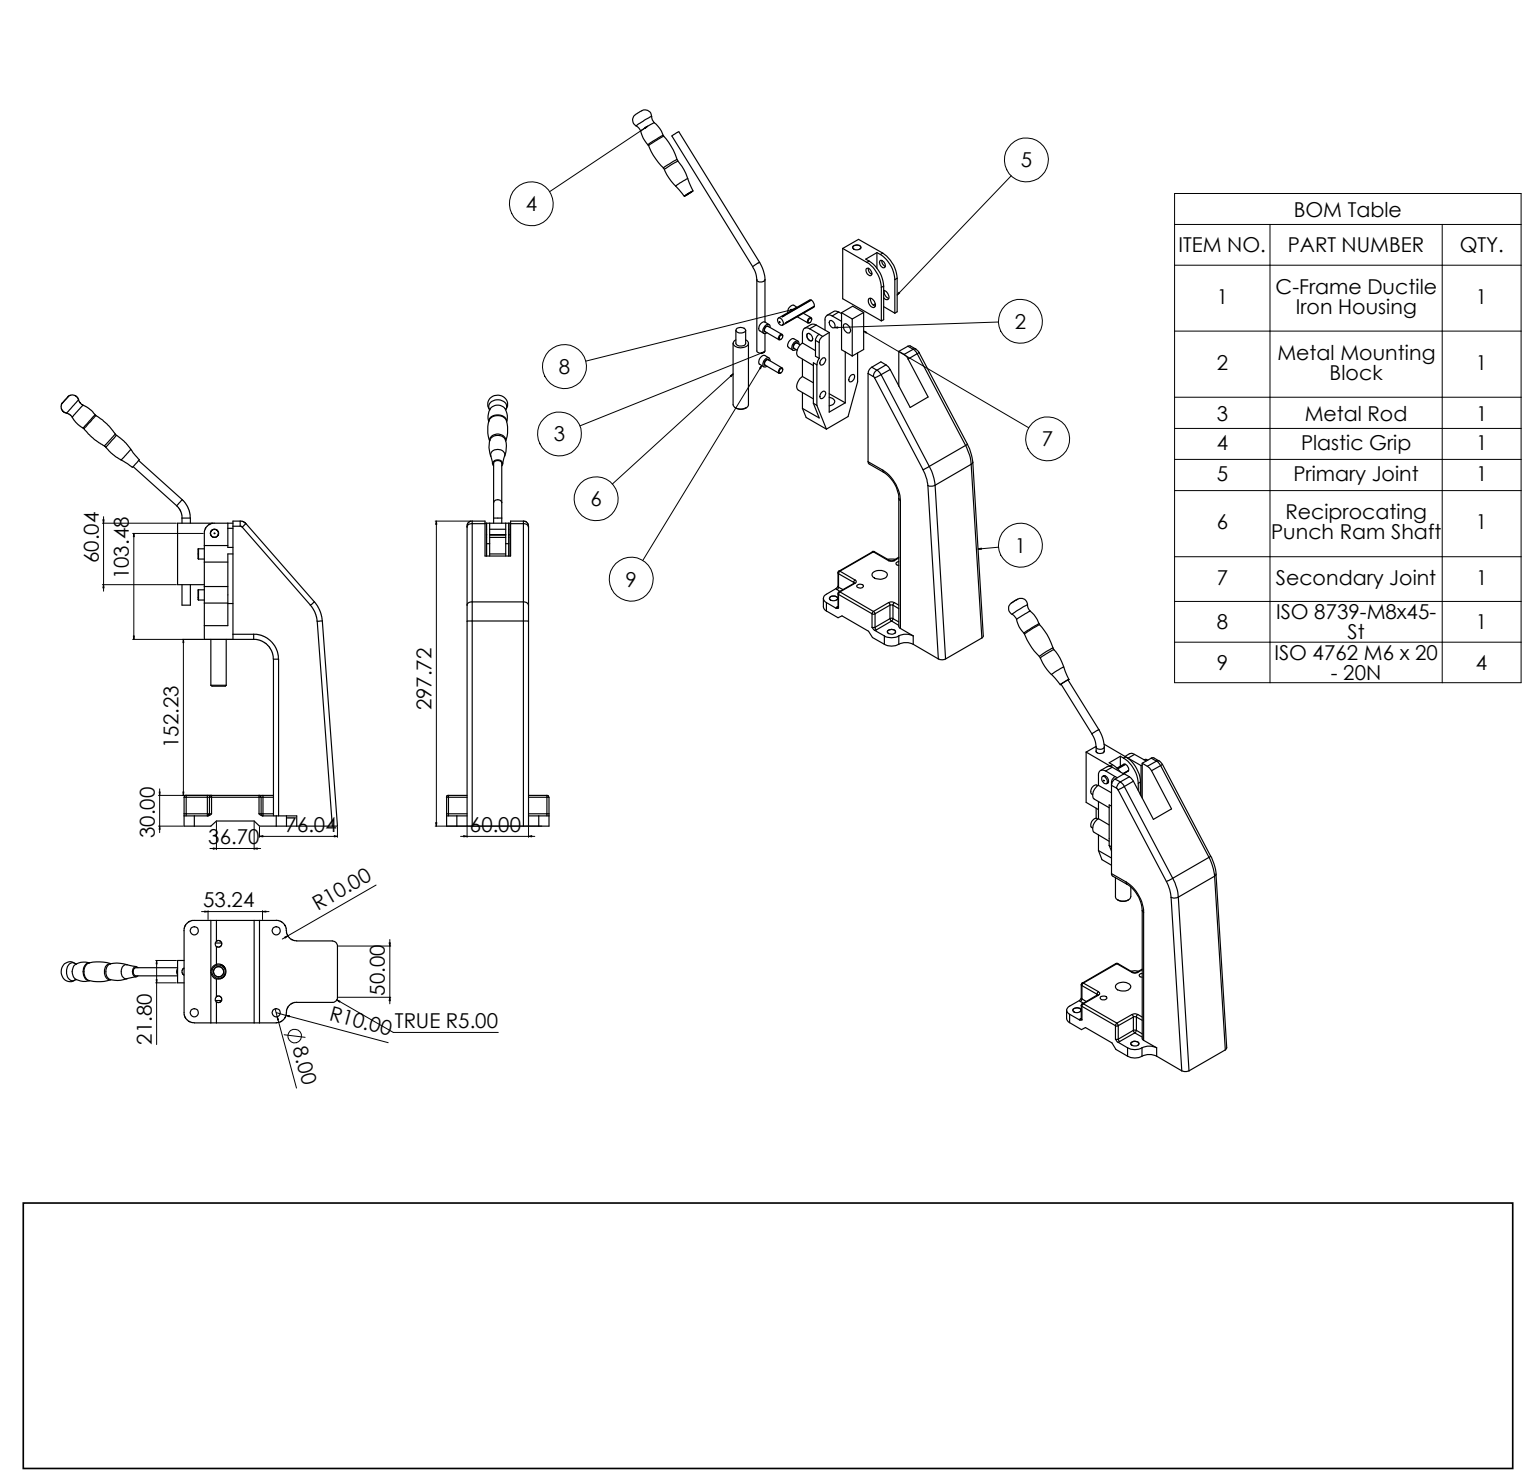
ISO-10303-21;
HEADER;
FILE_DESCRIPTION (('STEP AP214'),
    '1' );
FILE_NAME ('MAS-316',
    '2026-10-20T14:49:59',
    ( '' ),
    ( '' ),
    'SwSTEP 2.0',
    'SolidWorks 2025',
    '' );
FILE_SCHEMA (( 'AUTOMOTIVE_DESIGN' ));
ENDSEC;

DATA;
#1 = AXIS2_PLACEMENT_3D ( 'NONE', #1947, #6240, #1422 ) ;
#2 = CARTESIAN_POINT ( 'NONE',  ( 3.000000000000000000, 2.935248768560057897, -3.252606517456513302E-15 ) ) ;
#3 = LINE ( 'NONE', #5660, #7079 ) ;
#4 = DIRECTION ( 'NONE',  ( -0.6691306063588561281, -0.7431448254773960205, 0.000000000000000000 ) ) ;
#5 =( BOUNDED_CURVE ( )  B_SPLINE_CURVE ( 3, ( #4259, #2824, #7496, #242 ),
 .UNSPECIFIED., .F., .F. ) 
 B_SPLINE_CURVE_WITH_KNOTS ( ( 4, 4 ),
 ( 3.228493165690314637, 4.434806757669079502 ),
 .UNSPECIFIED. ) 
 CURVE ( )  GEOMETRIC_REPRESENTATION_ITEM ( )  RATIONAL_B_SPLINE_CURVE ( ( 1.000000000000000000, 0.8823660295963204891, 0.8823660295963204891, 1.000000000000000000 ) ) 
 REPRESENTATION_ITEM ( '' )  );
#6 = ORIENTED_EDGE ( 'NONE', *, *, #7618, .F. ) ;
#7 = EDGE_CURVE ( 'NONE', #389, #4565, #2197, .T. ) ;
#8 = VERTEX_POINT ( 'NONE', #6223 ) ;
#9 = ORIENTED_EDGE ( 'NONE', *, *, #9037, .T. ) ;
#10 = FACE_BOUND ( 'NONE', #10352, .T. ) ;
#11 = CARTESIAN_POINT ( 'NONE',  ( -47.94539818030330025, 137.0132282531173473, 3.999999999999991562 ) ) ;
#12 = DIRECTION ( 'NONE',  ( 0.000000000000000000, 0.000000000000000000, 1.000000000000000000 ) ) ;
#13 = VERTEX_POINT ( 'NONE', #5217 ) ;
#14 = DIRECTION ( 'NONE',  ( -0.6691306063588562392, -0.7431448254773959095, 0.000000000000000000 ) ) ;
#15 = ORIENTED_EDGE ( 'NONE', *, *, #8479, .F. ) ;
#16 = DIRECTION ( 'NONE',  ( -0.6691306063588565722, -0.7431448254773957984, 0.000000000000000000 ) ) ;
#17 = EDGE_CURVE ( 'NONE', #7054, #8863, #10257, .T. ) ;
#18 = ORIENTED_EDGE ( 'NONE', *, *, #2489, .T. ) ;
#19 = VECTOR ( 'NONE', #6137, 1000.000000000000114 ) ;
#20 = ORIENTED_EDGE ( 'NONE', *, *, #4444, .T. ) ;
#21 = DIRECTION ( 'NONE',  ( -1.000000000000000000, 0.000000000000000000, -1.396588258780021135E-16 ) ) ;
#22 = FACE_OUTER_BOUND ( 'NONE', #5382, .T. ) ;
#23 = PRODUCT_DEFINITION_SHAPE ( 'NONE', 'NONE',  #10488 ) ;
#24 = DIRECTION ( 'NONE',  ( 0.000000000000000000, -1.000000000000000000, -9.100899318238107179E-17 ) ) ;
#25 = DIRECTION ( 'NONE',  ( -1.000000000000000000, 0.000000000000000000, 0.000000000000000000 ) ) ;
#26 = AXIS2_PLACEMENT_3D ( 'NONE', #141, #5845, #6542 ) ;
#27 = ORIENTED_EDGE ( 'NONE', *, *, #3979, .T. ) ;
#28 = VECTOR ( 'NONE', #9785, 1000.000000000000000 ) ;
#29 = CARTESIAN_POINT ( 'NONE',  ( 3.000000000000000000, 0.000000000000000000, 0.000000000000000000 ) ) ;
#30 = ADVANCED_FACE ( 'NONE', ( #9249 ), #6112, .F. ) ;
#31 = EDGE_CURVE ( 'NONE', #2894, #7105, #9463, .T. ) ;
#32 = EDGE_CURVE ( 'NONE', #6206, #5311, #7708, .T. ) ;
#33 = CONTEXT_DEPENDENT_SHAPE_REPRESENTATION ( #9797, #23 ) ;
#34 = VERTEX_POINT ( 'NONE', #5261 ) ;
#35 = DIRECTION ( 'NONE',  ( 1.000000000000000000, -0.000000000000000000, -0.000000000000000000 ) ) ;
#36 = VERTEX_POINT ( 'NONE', #6165 ) ;
#37 = CIRCLE ( 'NONE', #7311, 10.00000000000000178 ) ;
#38 = AXIS2_PLACEMENT_3D ( 'NONE', #7742, #2701, #6091 ) ;
#39 = VERTEX_POINT ( 'NONE', #5423 ) ;
#40 = CARTESIAN_POINT ( 'NONE',  ( 2.108096605167895612E-14, -117.1457019118819005, -25.15769640663941686 ) ) ;
#41 = CARTESIAN_POINT ( 'NONE',  ( -7.293506896408097795, 145.5696653505793563, -20.00000000000000711 ) ) ;
#42 = CARTESIAN_POINT ( 'NONE',  ( 39.99999999999998579, -135.1707019118818778, -36.00000000000002842 ) ) ;
#43 = DIRECTION ( 'NONE',  ( -1.000000000000000000, 0.000000000000000000, 0.000000000000000000 ) ) ;
#44 = LINE ( 'NONE', #8251, #3603 ) ;
#45 = VECTOR ( 'NONE', #8925, 1000.000000000000000 ) ;
#46 = EDGE_CURVE ( 'NONE', #9808, #836, #8928, .T. ) ;
#47 = VERTEX_POINT ( 'NONE', #6006 ) ;
#48 = CARTESIAN_POINT ( 'NONE',  ( -16.29350689640809691, -186.9457019118818835, 23.72119897386845722 ) ) ;
#49 = ORIENTED_EDGE ( 'NONE', *, *, #1262, .T. ) ;
#50 = DIRECTION ( 'NONE',  ( 1.000000000000000000, 0.000000000000000000, -1.734723475976805615E-16 ) ) ;
#51 = CYLINDRICAL_SURFACE ( 'NONE', #8825, 4.000000000000000000 ) ;
#52 = AXIS2_PLACEMENT_3D ( 'NONE', #3037, #3895, #4040 ) ;
#53 =( NAMED_UNIT ( * ) SI_UNIT ( $, .STERADIAN. ) SOLID_ANGLE_UNIT ( ) );
#54 = AXIS2_PLACEMENT_3D ( 'NONE', #4576, #604, #662 ) ;
#55 = DIRECTION ( 'NONE',  ( -0.7367503238654704578, -0.6761648913424330720, -0.000000000000000000 ) ) ;
#56 = CARTESIAN_POINT ( 'NONE',  ( 99.80027788547049283, -145.1457019118819574, 25.00000000000000000 ) ) ;
#57 = LINE ( 'NONE', #8266, #434 ) ;
#58 = ORIENTED_EDGE ( 'NONE', *, *, #5513, .T. ) ;
#59 = VERTEX_POINT ( 'NONE', #6862 ) ;
#60 = ORIENTED_EDGE ( 'NONE', *, *, #10146, .T. ) ;
#61 = AXIS2_PLACEMENT_3D ( 'NONE', #1587, #8044, #3822 ) ;
#62 = ORIENTED_EDGE ( 'NONE', *, *, #3204, .F. ) ;
#63 = CARTESIAN_POINT ( 'NONE',  ( -47.94539818030330025, 150.5696653505793563, 3.999999999999993339 ) ) ;
#64 = ADVANCED_FACE ( 'NONE', ( #10099 ), #3860, .F. ) ;
#65 = DIRECTION ( 'NONE',  ( -0.000000000000000000, -0.000000000000000000, -1.000000000000000000 ) ) ;
#66 = LINE ( 'NONE', #8964, #2259 ) ;
#67 = DIRECTION ( 'NONE',  ( -0.7071067811864983899, 8.659560562354331352E-17, 0.7071067811865966446 ) ) ;
#68 = CIRCLE ( 'NONE', #1421, 4.025000000000000355 ) ;
#69 = ORIENTED_EDGE ( 'NONE', *, *, #7396, .F. ) ;
#70 = FACE_OUTER_BOUND ( 'NONE', #3100, .T. ) ;
#71 = VECTOR ( 'NONE', #3438, 1000.000000000000000 ) ;
#72 = ORIENTED_EDGE ( 'NONE', *, *, #1454, .F. ) ;
#73 = CIRCLE ( 'NONE', #8358, 4.025000000000000355 ) ;
#74 = ORIENTED_EDGE ( 'NONE', *, *, #80, .F. ) ;
#75 = UNCERTAINTY_MEASURE_WITH_UNIT (LENGTH_MEASURE( 1.000000000000000082E-05 ), #6894, 'distance_accuracy_value', 'NONE');
#76 = ORIENTED_EDGE ( 'NONE', *, *, #6234, .T. ) ;
#77 = DIRECTION ( 'NONE',  ( -1.000000000000000000, 0.000000000000000000, 0.000000000000000000 ) ) ;
#78 = DIRECTION ( 'NONE',  ( 0.000000000000000000, 1.000000000000000000, -1.329743448921560837E-15 ) ) ;
#79 = LINE ( 'NONE', #3304, #8495 ) ;
#80 = EDGE_CURVE ( 'NONE', #1253, #6094, #1141, .T. ) ;
#81 = DIRECTION ( 'NONE',  ( 0.000000000000000000, 1.000000000000000000, 0.000000000000000000 ) ) ;
#82 = LINE ( 'NONE', #7283, #1628 ) ;
#83 = CIRCLE ( 'NONE', #590, 5.025000000000002132 ) ;
#84 = VERTEX_POINT ( 'NONE', #3844 ) ;
#85 = DIRECTION ( 'NONE',  ( 0.000000000000000000, 0.000000000000000000, -1.000000000000000000 ) ) ;
#86 = VERTEX_POINT ( 'NONE', #4732 ) ;
#87 = CARTESIAN_POINT ( 'NONE',  ( 37.22511195853866894, 17.84145331825995484, -25.00000000000000355 ) ) ;
#88 = ORIENTED_EDGE ( 'NONE', *, *, #32, .T. ) ;
#89 = ADVANCED_FACE ( 'NONE', ( #9520 ), #9630, .T. ) ;
#90 = ADVANCED_FACE ( 'NONE', ( #4832 ), #5200, .F. ) ;
#91 = DIRECTION ( 'NONE',  ( 0.000000000000000000, -1.222897680782651471E-16, 1.000000000000000000 ) ) ;
#92 = AXIS2_PLACEMENT_3D ( 'NONE', #1690, #1849, #8953 ) ;
#93 = DIRECTION ( 'NONE',  ( 0.000000000000000000, -0.000000000000000000, -1.000000000000000000 ) ) ;
#94 = FACE_OUTER_BOUND ( 'NONE', #233, .T. ) ;
#95 = DIRECTION ( 'NONE',  ( -0.000000000000000000, -0.000000000000000000, 1.000000000000000000 ) ) ;
#96 = DIRECTION ( 'NONE',  ( 0.000000000000000000, 0.000000000000000000, 1.000000000000000000 ) ) ;
#97 = EDGE_LOOP ( 'NONE', ( #5379, #7947, #3762, #7012 ) ) ;
#98 = LINE ( 'NONE', #6716, #4014 ) ;
#99 = ORIENTED_EDGE ( 'NONE', *, *, #5544, .F. ) ;
#100 = LINE ( 'NONE', #5018, #2677 ) ;
#101 = EDGE_CURVE ( 'NONE', #6753, #3816, #8421, .T. ) ;
#102 = CYLINDRICAL_SURFACE ( 'NONE', #1212, 2.000000000000001776 ) ;
#103 = EDGE_CURVE ( 'NONE', #7113, #7038, #645, .T. ) ;
#104 = VECTOR ( 'NONE', #4491, 1000.000000000000000 ) ;
#105 = EDGE_CURVE ( 'NONE', #8005, #7120, #1404, .T. ) ;
#106 = DIRECTION ( 'NONE',  ( -1.000000000000000000, -0.000000000000000000, -0.000000000000000000 ) ) ;
#107 = DIRECTION ( 'NONE',  ( 0.000000000000000000, 0.000000000000000000, 1.000000000000000000 ) ) ;
#108 = DIRECTION ( 'NONE',  ( 1.000000000000000000, 0.000000000000000000, 0.000000000000000000 ) ) ;
#109 = VERTEX_POINT ( 'NONE', #7181 ) ;
#110 = ORIENTED_EDGE ( 'NONE', *, *, #8315, .T. ) ;
#111 = ORIENTED_EDGE ( 'NONE', *, *, #371, .T. ) ;
#112 = AXIS2_PLACEMENT_3D ( 'NONE', #10075, #7738, #3660 ) ;
#113 = VECTOR ( 'NONE', #5634, 1000.000000000000000 ) ;
#114 = ORIENTED_EDGE ( 'NONE', *, *, #3993, .T. ) ;
#115 = ORIENTED_EDGE ( 'NONE', *, *, #7748, .F. ) ;
#116 = DIRECTION ( 'NONE',  ( 0.000000000000000000, 0.000000000000000000, 1.000000000000000000 ) ) ;
#117 =( NAMED_UNIT ( * ) SI_UNIT ( $, .STERADIAN. ) SOLID_ANGLE_UNIT ( ) );
#118 = EDGE_CURVE ( 'NONE', #991, #7873, #6383, .T. ) ;
#119 = DIRECTION ( 'NONE',  ( -0.000000000000000000, 1.000000000000000000, -0.000000000000000000 ) ) ;
#120 = DIRECTION ( 'NONE',  ( -0.000000000000000000, 1.000000000000000000, -0.000000000000000000 ) ) ;
#121 = VECTOR ( 'NONE', #5228, 1000.000000000000000 ) ;
#122 = ORIENTED_EDGE ( 'NONE', *, *, #3348, .T. ) ;
#123 = DIRECTION ( 'NONE',  ( -0.000000000000000000, 1.000000000000000000, -0.000000000000000000 ) ) ;
#124 = CIRCLE ( 'NONE', #1803, 7.500000000000000000 ) ;
#125 = VERTEX_POINT ( 'NONE', #7868 ) ;
#126 = VECTOR ( 'NONE', #3375, 1000.000000000000000 ) ;
#127 = CARTESIAN_POINT ( 'NONE',  ( 39.99999999999998579, -115.1457019118818863, -50.00000000000002132 ) ) ;
#128 = EDGE_CURVE ( 'NONE', #9477, #9534, #1310, .T. ) ;
#129 = VECTOR ( 'NONE', #2614, 1000.000000000000000 ) ;
#130 = ORIENTED_EDGE ( 'NONE', *, *, #2088, .F. ) ;
#131 = ORIENTED_EDGE ( 'NONE', *, *, #6804, .F. ) ;
#132 = DIRECTION ( 'NONE',  ( -0.7431448254773957984, 0.6691306063588565722, -0.000000000000000000 ) ) ;
#133 = ADVANCED_BREP_SHAPE_REPRESENTATION ( '', ( #10321, #4601 ), #2278 ) ;
#134 = CIRCLE ( 'NONE', #4024, 3.999999999999993339 ) ;
#135 = DIRECTION ( 'NONE',  ( 0.000000000000000000, 0.000000000000000000, -1.000000000000000000 ) ) ;
#136 = CARTESIAN_POINT ( 'NONE',  ( -16.29350689640809691, -8.635287962196477096, 0.000000000000000000 ) ) ;
#137 = DIRECTION ( 'NONE',  ( 0.000000000000000000, 0.000000000000000000, 1.000000000000000000 ) ) ;
#138 = CARTESIAN_POINT ( 'NONE',  ( -7.293506896408097795, 50.54838324668256888, 20.00000000000001776 ) ) ;
#139 = VECTOR ( 'NONE', #10142, 1000.000000000000000 ) ;
#140 = ORIENTED_EDGE ( 'NONE', *, *, #5070, .F. ) ;
#141 = CARTESIAN_POINT ( 'NONE',  ( -23.17384457509314899, 130.5696653505793847, 10.90000000000000036 ) ) ;
#142 = EDGE_CURVE ( 'NONE', #5755, #3381, #6273, .T. ) ;
#143 = ORIENTED_EDGE ( 'NONE', *, *, #3330, .T. ) ;
#144 = DIRECTION ( 'NONE',  ( -1.000000000000000000, 0.000000000000000000, 0.000000000000000000 ) ) ;
#145 = ORIENTED_EDGE ( 'NONE', *, *, #5104, .T. ) ;
#146 = AXIS2_PLACEMENT_3D ( 'NONE', #654, #6367, #4769 ) ;
#147 = SHAPE_REPRESENTATION_RELATIONSHIP ( 'NONE' , 'NONE' ,  #7587, #133 ) ;
#148 = FACE_OUTER_BOUND ( 'NONE', #7245, .T. ) ;
#149 = AXIS2_PLACEMENT_3D ( 'NONE', #5640, #2363, #7980 ) ;
#150 = FACE_BOUND ( 'NONE', #8598, .T. ) ;
#151 = FACE_OUTER_BOUND ( 'NONE', #4068, .T. ) ;
#152 = FACE_OUTER_BOUND ( 'NONE', #4686, .T. ) ;
#153 = DIRECTION ( 'NONE',  ( -1.000000000000000000, 0.000000000000000000, 0.000000000000000000 ) ) ;
#154 = AXIS2_PLACEMENT_3D ( 'NONE', #9604, #3022, #736 ) ;
#155 = EDGE_CURVE ( 'NONE', #5994, #6514, #9956, .T. ) ;
#156 = ORIENTED_EDGE ( 'NONE', *, *, #9691, .F. ) ;
#157 = CARTESIAN_POINT ( 'NONE',  ( -2.293506896408097795, 120.5696653505793705, 20.00000000000000711 ) ) ;
#158 = CIRCLE ( 'NONE', #4883, 4.982234098198590644 ) ;
#159 = ORIENTED_EDGE ( 'NONE', *, *, #5597, .F. ) ;
#160 = CARTESIAN_POINT ( 'NONE',  ( -2.293506896408097795, 120.5696653505793705, 16.00000000000000711 ) ) ;
#161 = FACE_OUTER_BOUND ( 'NONE', #8002, .T. ) ;
#162 = DIRECTION ( 'NONE',  ( 0.000000000000000000, 0.000000000000000000, -1.000000000000000000 ) ) ;
#163 = CARTESIAN_POINT ( 'NONE',  ( 0.000000000000000000, -135.1457019118818721, 49.99999999999997868 ) ) ;
#164 = DIRECTION ( 'NONE',  ( -0.000000000000000000, 1.000000000000000000, -0.000000000000000000 ) ) ;
#165 = DIRECTION ( 'NONE',  ( 1.000000000000000000, 0.000000000000000000, -0.000000000000000000 ) ) ;
#166 = CONICAL_SURFACE ( 'NONE', #1514, 4.025000000000000355, 0.7853981633977258348 ) ;
#167 = ORIENTED_EDGE ( 'NONE', *, *, #1641, .F. ) ;
#168 = ADVANCED_FACE ( 'NONE', ( #10363, #4632, #9677 ), #1511, .F. ) ;
#169 = EDGE_CURVE ( 'NONE', #490, #9911, #7578, .T. ) ;
#170 = EDGE_LOOP ( 'NONE', ( #1521, #9934, #3722, #2301 ) ) ;
#171 = EDGE_CURVE ( 'NONE', #8144, #3030, #5631, .T. ) ;
#172 = VERTEX_POINT ( 'NONE', #5530 ) ;
#173 = DIRECTION ( 'NONE',  ( 1.000000000000000000, 0.000000000000000000, 0.000000000000000000 ) ) ;
#174 = CARTESIAN_POINT ( 'NONE',  ( 4.856471286862176662, 145.0444252872335937, -25.00000000000000355 ) ) ;
#175 = CARTESIAN_POINT ( 'NONE',  ( 39.99999999999998579, -135.1707019118818778, -40.00000000000002132 ) ) ;
#176 = ORIENTED_EDGE ( 'NONE', *, *, #2184, .F. ) ;
#177 = DIRECTION ( 'NONE',  ( -8.194486552889013533E-17, -9.100899318238110877E-17, 1.000000000000000000 ) ) ;
#178 = ORIENTED_EDGE ( 'NONE', *, *, #10204, .T. ) ;
#179 = DIRECTION ( 'NONE',  ( -0.6691306063588574604, -0.7431448254773949103, 0.000000000000000000 ) ) ;
#180 = ADVANCED_FACE ( 'NONE', ( #7280 ), #10317, .T. ) ;
#181 = ORIENTED_EDGE ( 'NONE', *, *, #259, .T. ) ;
#182 = PRODUCT_DEFINITION_CONTEXT ( 'detailed design', #6258, 'design' ) ;
#183 = CARTESIAN_POINT ( 'NONE',  ( -147.2606667696710474, 253.8574007319445229, 0.000000000000000000 ) ) ;
#184 = DIRECTION ( 'NONE',  ( 0.6761648913424331830, 0.7367503238654705688, 0.000000000000000000 ) ) ;
#185 = FACE_OUTER_BOUND ( 'NONE', #1495, .T. ) ;
#186 = CARTESIAN_POINT ( 'NONE',  ( -8.793506896408096907, 120.5289575273812233, 54.43095569077609497 ) ) ;
#187 = PLANE ( 'NONE',  #9912 ) ;
#188 = CARTESIAN_POINT ( 'NONE',  ( -30.29350689640809335, 37.08684478514406635, 0.000000000000000000 ) ) ;
#189 = ORIENTED_EDGE ( 'NONE', *, *, #3670, .T. ) ;
#190 = CARTESIAN_POINT ( 'NONE',  ( -7.293506896408097795, 50.54838324668256888, -20.00000000000001776 ) ) ;
#191 = AXIS2_PLACEMENT_3D ( 'NONE', #9432, #5392, #4342 ) ;
#192 = PRODUCT_CONTEXT ( 'NONE', #5163, 'mechanical' ) ;
#193 = ORIENTED_EDGE ( 'NONE', *, *, #118, .T. ) ;
#194 = CARTESIAN_POINT ( 'NONE',  ( 0.000000000000000000, -135.1457019118818721, 0.000000000000000000 ) ) ;
#195 = VERTEX_POINT ( 'NONE', #3902 ) ;
#196 = ADVANCED_FACE ( 'NONE', ( #3094 ), #2303, .F. ) ;
#197 = DIRECTION ( 'NONE',  ( -0.6691306063588565722, -0.7431448254773959095, 0.000000000000000000 ) ) ;
#198 = AXIS2_PLACEMENT_3D ( 'NONE', #3567, #10035, #1182 ) ;
#199 = DIRECTION ( 'NONE',  ( 0.000000000000000000, 0.000000000000000000, -1.000000000000000000 ) ) ;
#200 = DIRECTION ( 'NONE',  ( 0.000000000000000000, 1.000000000000000000, 0.000000000000000000 ) ) ;
#201 = DIRECTION ( 'NONE',  ( -0.000000000000000000, 1.000000000000000000, -0.000000000000000000 ) ) ;
#202 = DIRECTION ( 'NONE',  ( 0.000000000000000000, 0.000000000000000000, -1.000000000000000000 ) ) ;
#203 = EDGE_LOOP ( 'NONE', ( #8240, #8305, #10001, #6976, #3187, #9611 ) ) ;
#204 = AXIS2_PLACEMENT_3D ( 'NONE', #9863, #838, #6454 ) ;
#205 = CARTESIAN_POINT ( 'NONE',  ( -47.94539818030328604, 85.52895752738115220, 4.000000000000000000 ) ) ;
#206 = CIRCLE ( 'NONE', #9340, 5.000000000000000888 ) ;
#207 = EDGE_LOOP ( 'NONE', ( #1735, #9870, #2298, #4217 ) ) ;
#208 = DIRECTION ( 'NONE',  ( -0.000000000000000000, -0.000000000000000000, -1.000000000000000000 ) ) ;
#209 = FACE_OUTER_BOUND ( 'NONE', #8382, .T. ) ;
#210 = DIRECTION ( 'NONE',  ( 0.000000000000000000, -1.000000000000000000, 0.000000000000000000 ) ) ;
#211 = DIRECTION ( 'NONE',  ( 1.000000000000000000, 0.000000000000000000, 0.000000000000000000 ) ) ;
#212 = ADVANCED_FACE ( 'NONE', ( #4987 ), #7922, .T. ) ;
#213 = DIRECTION ( 'NONE',  ( -0.7431448254773957984, 0.6691306063588565722, -0.000000000000000000 ) ) ;
#214 = AXIS2_PLACEMENT_3D ( 'NONE', #6935, #10169, #2741 ) ;
#215 = CARTESIAN_POINT ( 'NONE',  ( 39.99999999999997158, -135.1707019118818778, 35.99999999999998579 ) ) ;
#216 = ORIENTED_EDGE ( 'NONE', *, *, #1932, .F. ) ;
#217 = ORIENTED_EDGE ( 'NONE', *, *, #8260, .F. ) ;
#218 = VECTOR ( 'NONE', #1908, 1000.000000000000000 ) ;
#219 = ORIENTED_EDGE ( 'NONE', *, *, #8508, .T. ) ;
#220 = CIRCLE ( 'NONE', #5954, 2.000000000000001776 ) ;
#221 = CARTESIAN_POINT ( 'NONE',  ( -0.8557715602033003632, -3.117691453623970599, -1.800000000000014921 ) ) ;
#222 = DIRECTION ( 'NONE',  ( 1.000000000000000000, -0.000000000000000000, -0.000000000000000000 ) ) ;
#223 = ADVANCED_FACE ( 'NONE', ( #968 ), #9262, .F. ) ;
#224 = CARTESIAN_POINT ( 'NONE',  ( -30.29350689640809335, 80.56966535057935630, -24.00000000000000711 ) ) ;
#225 = EDGE_CURVE ( 'NONE', #5542, #7357, #9074, .T. ) ;
#226 = ORIENTED_EDGE ( 'NONE', *, *, #6379, .T. ) ;
#227 = CARTESIAN_POINT ( 'NONE',  ( 14.70649310359190309, 120.5696653505793705, 20.00000000000000711 ) ) ;
#228 = TOROIDAL_SURFACE ( 'NONE', #6479, 2.525240063345735475, 5.000000000000000000 ) ;
#229 = ORIENTED_EDGE ( 'NONE', *, *, #1078, .F. ) ;
#230 = CARTESIAN_POINT ( 'NONE',  ( 14.70649310359190309, 120.5696653505793705, 20.00000000000000711 ) ) ;
#231 = ORIENTED_EDGE ( 'NONE', *, *, #934, .T. ) ;
#232 = ORIENTED_EDGE ( 'NONE', *, *, #10101, .T. ) ;
#233 = EDGE_LOOP ( 'NONE', ( #9990, #9923, #6076 ) ) ;
#234 = CARTESIAN_POINT ( 'NONE',  ( -40.00000000000001421, -145.1457019118819005, -40.00000000000002132 ) ) ;
#235 = VECTOR ( 'NONE', #6566, 1000.000000000000000 ) ;
#236 = DIRECTION ( 'NONE',  ( -1.000000000000000000, 0.000000000000000000, 9.101836848464096770E-17 ) ) ;
#237 = DIRECTION ( 'NONE',  ( -0.7431448254773957984, 0.6691306063588565722, -0.000000000000000000 ) ) ;
#238 = ADVANCED_FACE ( 'NONE', ( #290 ), #4855, .T. ) ;
#239 = EDGE_CURVE ( 'NONE', #4318, #3843, #3408, .T. ) ;
#240 = EDGE_CURVE ( 'NONE', #10167, #8252, #4254, .T. ) ;
#241 = CARTESIAN_POINT ( 'NONE',  ( -142.3328939341254795, 249.4204141414382434, 0.000000000000000000 ) ) ;
#242 = CARTESIAN_POINT ( 'NONE',  ( -18.34874108452141783, -140.1746510883711778, 7.212905963064383918 ) ) ;
#243 = ORIENTED_EDGE ( 'NONE', *, *, #6508, .F. ) ;
#244 = CARTESIAN_POINT ( 'NONE',  ( -40.00000000000002842, -135.1457019118818721, 39.99999999999997868 ) ) ;
#245 = CIRCLE ( 'NONE', #4296, 4.024999999999997691 ) ;
#246 = ORIENTED_EDGE ( 'NONE', *, *, #9487, .F. ) ;
#247 = PRODUCT_DEFINITION_FORMATION_WITH_SPECIFIED_SOURCE ( 'ANY', '', #7048, .NOT_KNOWN. ) ;
#248 = LINE ( 'NONE', #2462, #7946 ) ;
#249 = VERTEX_POINT ( 'NONE', #5785 ) ;
#250 = AXIS2_PLACEMENT_3D ( 'NONE', #3199, #920, #4939 ) ;
#251 = EDGE_CURVE ( 'NONE', #7304, #5030, #3169, .T. ) ;
#252 = FACE_BOUND ( 'NONE', #5488, .T. ) ;
#253 = CARTESIAN_POINT ( 'NONE',  ( -50.00000000000002132, -115.1457019118818863, 23.15769640663938134 ) ) ;
#254 = CARTESIAN_POINT ( 'NONE',  ( -56.36957570605427748, 150.5696653505793563, 10.90000000000000036 ) ) ;
#255 = AXIS2_PLACEMENT_3D ( 'NONE', #5974, #6135, #9270 ) ;
#256 = DIRECTION ( 'NONE',  ( 0.000000000000000000, 0.000000000000000000, -1.000000000000000000 ) ) ;
#257 = CARTESIAN_POINT ( 'NONE',  ( -23.15769640663940976, -133.1457019118818721, 49.99999999999997868 ) ) ;
#258 = DIRECTION ( 'NONE',  ( 0.000000000000000000, 0.000000000000000000, 1.000000000000000000 ) ) ;
#259 = EDGE_CURVE ( 'NONE', #9948, #541, #8974, .T. ) ;
#260 = EDGE_LOOP ( 'NONE', ( #7752, #8876, #7839, #4575 ) ) ;
#261 = AXIS2_PLACEMENT_3D ( 'NONE', #3282, #9005, #108 ) ;
#262 = DIRECTION ( 'NONE',  ( 1.000000000000000000, 0.000000000000000000, 0.000000000000000000 ) ) ;
#263 = VECTOR ( 'NONE', #2110, 1000.000000000000000 ) ;
#264 = VERTEX_POINT ( 'NONE', #1663 ) ;
#265 = FACE_OUTER_BOUND ( 'NONE', #5639, .T. ) ;
#266 = DIRECTION ( 'NONE',  ( -0.000000000000000000, 1.000000000000000000, -0.000000000000000000 ) ) ;
#267 = B_SPLINE_CURVE_WITH_KNOTS ( 'NONE', 3,
 ( #1751, #6037, #5296, #7584 ),
 .UNSPECIFIED., .F., .F.,
 ( 4, 4 ),
 ( 0.000000000000000000, 0.0007942240325546930492 ),
 .UNSPECIFIED. ) ;
#268 = DIRECTION ( 'NONE',  ( -0.9805806756909200006, 0.000000000000000000, 0.1961161351381848494 ) ) ;
#269 = DIRECTION ( 'NONE',  ( 0.000000000000000000, 0.000000000000000000, -1.000000000000000000 ) ) ;
#270 = LINE ( 'NONE', #5923, #8481 ) ;
#271 = CIRCLE ( 'NONE', #8898, 4.999999999999997335 ) ;
#272 = ORIENTED_EDGE ( 'NONE', *, *, #9010, .T. ) ;
#273 = ORIENTED_EDGE ( 'NONE', *, *, #8937, .T. ) ;
#274 = EDGE_CURVE ( 'NONE', #9380, #1455, #6041, .T. ) ;
#275 = ORIENTED_EDGE ( 'NONE', *, *, #9151, .T. ) ;
#276 = CARTESIAN_POINT ( 'NONE',  ( -21.29350689640810046, 105.5289575273812233, -25.04213562373096380 ) ) ;
#277 = AXIS2_PLACEMENT_3D ( 'NONE', #10005, #5118, #7559 ) ;
#278 = DIRECTION ( 'NONE',  ( 0.000000000000000000, 0.000000000000000000, 1.000000000000000000 ) ) ;
#279 = FACE_OUTER_BOUND ( 'NONE', #7883, .T. ) ;
#280 = ORIENTED_EDGE ( 'NONE', *, *, #3281, .F. ) ;
#281 = CARTESIAN_POINT ( 'NONE',  ( -27.85255513972543895, 150.5696653505793563, -7.749999999999996447 ) ) ;
#282 = AXIS2_PLACEMENT_3D ( 'NONE', #1944, #4741, #724 ) ;
#283 = EDGE_LOOP ( 'NONE', ( #4736, #4335, #5874, #8256, #8188 ) ) ;
#284 = CYLINDRICAL_SURFACE ( 'NONE', #9989, 2.000000000000001776 ) ;
#285 = CIRCLE ( 'NONE', #7057, 3.999999999999996447 ) ;
#286 = SHAPE_REPRESENTATION ( 'Primary Joint', ( #4601 ), #409 ) ;
#287 = EDGE_CURVE ( 'NONE', #249, #2514, #5099, .T. ) ;
#288 = VERTEX_POINT ( 'NONE', #1021 ) ;
#289 = VERTEX_POINT ( 'NONE', #2558 ) ;
#290 = FACE_OUTER_BOUND ( 'NONE', #9585, .T. ) ;
#291 = SURFACE_SIDE_STYLE ('',( #8975 ) ) ;
#292 = AXIS2_PLACEMENT_3D ( 'NONE', #10403, #6319, #9565 ) ;
#293 = CARTESIAN_POINT ( 'NONE',  ( -48.00000000000002132, -133.1457019118818721, -27.15769640663945594 ) ) ;
#294 = FACE_OUTER_BOUND ( 'NONE', #1619, .T. ) ;
#295 = VECTOR ( 'NONE', #753, 1000.000000000000114 ) ;
#296 = DIRECTION ( 'NONE',  ( -0.000000000000000000, 1.000000000000000000, -0.000000000000000000 ) ) ;
#297 = CARTESIAN_POINT ( 'NONE',  ( 39.99999999999997158, -135.1457019118818721, 39.99999999999997868 ) ) ;
#298 = ORIENTED_EDGE ( 'NONE', *, *, #6850, .F. ) ;
#299 = DIRECTION ( 'NONE',  ( -8.194486552889013533E-17, -9.100899318238110877E-17, 1.000000000000000000 ) ) ;
#300 = EDGE_CURVE ( 'NONE', #1692, #6075, #1817, .T. ) ;
#302 = EDGE_CURVE ( 'NONE', #5556, #3604, #5045, .T. ) ;
#301 = ORIENTED_EDGE ( 'NONE', *, *, #542, .F. ) ;
#303 = EDGE_CURVE ( 'NONE', #4587, #5189, #10304, .T. ) ;
#304 = CARTESIAN_POINT ( 'NONE',  ( -39.66851723004002395, -4.408728476930471151E-16, 3.600000000000004530 ) ) ;
#305 = AXIS2_PLACEMENT_3D ( 'NONE', #4703, #7939, #5550 ) ;
#306 = ORIENTED_EDGE ( 'NONE', *, *, #8464, .F. ) ;
#307 = CLOSED_SHELL ( 'NONE', ( #4177, #2796, #9152, #8006, #10397, #7112, #488, #9693, #5992, #7606, #7526, #5005, #9842, #7992, #7050 ) ) ;
#308 = PLANE ( 'NONE',  #2610 ) ;
#309 = DIRECTION ( 'NONE',  ( -0.000000000000000000, -0.000000000000000000, 1.000000000000000000 ) ) ;
#310 = CARTESIAN_POINT ( 'NONE',  ( -40.33539666817951996, -3.418469287038251814, -2.079037510735993521 ) ) ;
#311 = EDGE_LOOP ( 'NONE', ( #929, #9154, #4963 ) ) ;
#312 = AXIS2_PLACEMENT_3D ( 'NONE', #483, #2971, #4458 ) ;
#313 = CARTESIAN_POINT ( 'NONE',  ( 53.40242741783141156, 42.08684478514406635, -30.00000000000000355 ) ) ;
#314 = CARTESIAN_POINT ( 'NONE',  ( 0.000000000000000000, 0.000000000000000000, 0.000000000000000000 ) ) ;
#315 = ORIENTED_EDGE ( 'NONE', *, *, #3953, .F. ) ;
#316 = VECTOR ( 'NONE', #2440, 1000.000000000000000 ) ;
#317 = EDGE_CURVE ( 'NONE', #10264, #2451, #2832, .T. ) ;
#318 = DIRECTION ( 'NONE',  ( 0.7431448254773962425, -0.6691306063588559061, 0.000000000000000000 ) ) ;
#319 = ORIENTED_EDGE ( 'NONE', *, *, #618, .T. ) ;
#320 = DIRECTION ( 'NONE',  ( -1.387778780781445676E-16, 0.000000000000000000, 1.000000000000000000 ) ) ;
#321 = DIRECTION ( 'NONE',  ( 0.000000000000000000, 0.000000000000000000, 1.000000000000000000 ) ) ;
#322 = CARTESIAN_POINT ( 'NONE',  ( -1.071796769724492338, 3.319229491889297279, -2.232199717805803285 ) ) ;
#323 = CARTESIAN_POINT ( 'NONE',  ( -38.19229777560033057, 37.08684478514405214, -12.50000000000000000 ) ) ;
#324 = DIRECTION ( 'NONE',  ( 6.106226635438360972E-16, -1.000000000000000000, 0.000000000000000000 ) ) ;
#325 = AXIS2_PLACEMENT_3D ( 'NONE', #7109, #9549, #7950 ) ;
#326 = CARTESIAN_POINT ( 'NONE',  ( -38.96131932220313132, -3.592756407884938330, -1.758437202063725779 ) ) ;
#327 = ORIENTED_EDGE ( 'NONE', *, *, #7111, .T. ) ;
#328 = ORIENTED_EDGE ( 'NONE', *, *, #6700, .F. ) ;
#329 = CARTESIAN_POINT ( 'NONE',  ( 14.70649310359190309, 120.5696653505793705, -20.00000000000000711 ) ) ;
#330 = CIRCLE ( 'NONE', #4045, 4.000000000000000000 ) ;
#331 = LINE ( 'NONE', #7790, #7501 ) ;
#332 = EDGE_CURVE ( 'NONE', #8658, #7935, #9280, .T. ) ;
#333 = CARTESIAN_POINT ( 'NONE',  ( -16.29350689640809691, 81.26698356513965393, -4.729641367753003145 ) ) ;
#334 = ORIENTED_EDGE ( 'NONE', *, *, #6698, .T. ) ;
#335 = DIRECTION ( 'NONE',  ( 0.000000000000000000, 0.000000000000000000, 1.000000000000000000 ) ) ;
#336 = ORIENTED_EDGE ( 'NONE', *, *, #3079, .T. ) ;
#337 = CARTESIAN_POINT ( 'NONE',  ( 14.70649310359190309, 80.56966535057935630, -20.00000000000000711 ) ) ;
#338 = CIRCLE ( 'NONE', #9475, 4.000000000000003553 ) ;
#339 = ORIENTED_EDGE ( 'NONE', *, *, #9708, .F. ) ;
#340 = ORIENTED_EDGE ( 'NONE', *, *, #1843, .F. ) ;
#341 = CARTESIAN_POINT ( 'NONE',  ( -152.9991366487805067, 270.9406871569508439, 1.084494555200859138E-15 ) ) ;
#342 = DIRECTION ( 'NONE',  ( 0.000000000000000000, 0.000000000000000000, -1.000000000000000000 ) ) ;
#343 = DIRECTION ( 'NONE',  ( 1.000000000000000000, 0.000000000000000000, -9.101836848464095537E-17 ) ) ;
#344 = DIRECTION ( 'NONE',  ( 1.000000000000000000, -0.000000000000000000, -0.000000000000000000 ) ) ;
#345 = ADVANCED_FACE ( 'NONE', ( #9025 ), #8120, .T. ) ;
#346 = CARTESIAN_POINT ( 'NONE',  ( 37.22797271129282848, -133.4137847133962396, -25.17122046401099311 ) ) ;
#347 = EDGE_LOOP ( 'NONE', ( #2435, #5782, #9896, #402 ) ) ;
#348 = DIRECTION ( 'NONE',  ( 0.000000000000000000, 1.000000000000000000, -0.000000000000000000 ) ) ;
#349 = ORIENTED_EDGE ( 'NONE', *, *, #1530, .T. ) ;
#350 = CARTESIAN_POINT ( 'NONE',  ( -3.173844575093148990, 90.52895752738122326, -7.750000000000000000 ) ) ;
#351 = CARTESIAN_POINT ( 'NONE',  ( 39.99999999999998579, -135.1457019118818721, -40.00000000000002132 ) ) ;
#352 = DIRECTION ( 'NONE',  ( 0.000000000000000000, 0.000000000000000000, 1.000000000000000000 ) ) ;
#353 = CYLINDRICAL_SURFACE ( 'NONE', #7185, 4.000000000000000000 ) ;
#354 = EDGE_CURVE ( 'NONE', #6075, #9366, #9784, .T. ) ;
#355 = CYLINDRICAL_SURFACE ( 'NONE', #5843, 4.000000000000000000 ) ;
#356 = EDGE_CURVE ( 'NONE', #5466, #9263, #915, .T. ) ;
#357 = EDGE_CURVE ( 'NONE', #2439, #4517, #2671, .T. ) ;
#358 = DIRECTION ( 'NONE',  ( -0.000000000000000000, -1.000000000000000000, -0.000000000000000000 ) ) ;
#359 = ORIENTED_EDGE ( 'NONE', *, *, #6276, .F. ) ;
#360 = DIRECTION ( 'NONE',  ( -0.000000000000000000, 1.000000000000000000, -0.000000000000000000 ) ) ;
#361 = EDGE_LOOP ( 'NONE', ( #8543, #5301 ) ) ;
#362 = DIRECTION ( 'NONE',  ( 1.000000000000000000, 0.000000000000000000, 0.000000000000000000 ) ) ;
#363 = EDGE_LOOP ( 'NONE', ( #8107, #2438, #3383, #9676 ) ) ;
#364 = DIRECTION ( 'NONE',  ( 0.000000000000000000, 0.8660254037844379305, -0.5000000000000012212 ) ) ;
#365 = CIRCLE ( 'NONE', #1375, 5.000000000000007994 ) ;
#366 = ORIENTED_EDGE ( 'NONE', *, *, #3251, .T. ) ;
#367 = DIRECTION ( 'NONE',  ( 1.000000000000000000, 0.000000000000000000, 0.000000000000000000 ) ) ;
#368 = FACE_OUTER_BOUND ( 'NONE', #3797, .T. ) ;
#369 = DIRECTION ( 'NONE',  ( 0.000000000000000000, 1.224646799147353207E-16, -1.000000000000000000 ) ) ;
#370 = FACE_OUTER_BOUND ( 'NONE', #8957, .T. ) ;
#371 = EDGE_CURVE ( 'NONE', #6079, #5542, #9235, .T. ) ;
#372 = CARTESIAN_POINT ( 'NONE',  ( -20.29350689640809691, 140.5696653505793563, 20.00000000000002132 ) ) ;
#373 = EDGE_CURVE ( 'NONE', #3710, #6945, #2925, .T. ) ;
#374 = VECTOR ( 'NONE', #4417, 1000.000000000000000 ) ;
#375 = ORIENTED_EDGE ( 'NONE', *, *, #6294, .F. ) ;
#376 = AXIS2_PLACEMENT_3D ( 'NONE', #9836, #6639, #8122 ) ;
#377 = ORIENTED_EDGE ( 'NONE', *, *, #2708, .T. ) ;
#378 = DIRECTION ( 'NONE',  ( 1.137729606058012035E-16, 0.000000000000000000, 1.000000000000000000 ) ) ;
#379 =( GEOMETRIC_REPRESENTATION_CONTEXT ( 3 ) GLOBAL_UNCERTAINTY_ASSIGNED_CONTEXT ( ( #4097 ) ) GLOBAL_UNIT_ASSIGNED_CONTEXT ( ( #7158, #2376, #5505 ) ) REPRESENTATION_CONTEXT ( 'NONE', 'WORKASPACE' ) );
#380 = DIRECTION ( 'NONE',  ( -9.101836848464095537E-17, -0.000000000000000000, -1.000000000000000000 ) ) ;
#381 = LINE ( 'NONE', #2917, #3516 ) ;
#382 = VERTEX_POINT ( 'NONE', #6794 ) ;
#383 = ORIENTED_EDGE ( 'NONE', *, *, #664, .T. ) ;
#384 = DIRECTION ( 'NONE',  ( -1.000000000000000000, -0.000000000000000000, -0.000000000000000000 ) ) ;
#385 = AXIS2_PLACEMENT_3D ( 'NONE', #470, #266, #3704 ) ;
#386 = AXIS2_PLACEMENT_3D ( 'NONE', #4274, #4902, #96 ) ;
#387 = EDGE_CURVE ( 'NONE', #9162, #3341, #2763, .T. ) ;
#388 = ORIENTED_EDGE ( 'NONE', *, *, #4709, .T. ) ;
#389 = VERTEX_POINT ( 'NONE', #6099 ) ;
#390 = DIRECTION ( 'NONE',  ( -0.000000000000000000, -0.000000000000000000, -1.000000000000000000 ) ) ;
#391 = LINE ( 'NONE', #7015, #708 ) ;
#392 = DIRECTION ( 'NONE',  ( -0.7525569905852185215, -0.6585271261848818503, 0.000000000000000000 ) ) ;
#393 = DIRECTION ( 'NONE',  ( -0.000000000000000000, -1.000000000000000000, -0.000000000000000000 ) ) ;
#394 = TOROIDAL_SURFACE ( 'NONE', #3944, 11.15107097094592881, 2.515249034521771510 ) ;
#395 = CIRCLE ( 'NONE', #5122, 2.541999999999999815 ) ;
#396 = DIRECTION ( 'NONE',  ( 9.101836848464095537E-17, 0.000000000000000000, 1.000000000000000000 ) ) ;
#397 = ORIENTED_EDGE ( 'NONE', *, *, #981, .F. ) ;
#398 = DIRECTION ( 'NONE',  ( 1.000000000000000000, -0.000000000000000000, -0.000000000000000000 ) ) ;
#399 = VECTOR ( 'NONE', #9659, 1000.000000000000000 ) ;
#400 = CARTESIAN_POINT ( 'NONE',  ( 99.80027788547049283, -145.1457019118819005, 25.00000000000000000 ) ) ;
#401 = EDGE_CURVE ( 'NONE', #2275, #493, #4466, .T. ) ;
#402 = ORIENTED_EDGE ( 'NONE', *, *, #1707, .F. ) ;
#403 = LINE ( 'NONE', #4479, #10289 ) ;
#404 = LINE ( 'NONE', #3533, #7016 ) ;
#405 = DIRECTION ( 'NONE',  ( -0.7431448254773957984, 0.6691306063588565722, -0.000000000000000000 ) ) ;
#406 = AXIS2_PLACEMENT_3D ( 'NONE', #8418, #9973, #3651 ) ;
#407 = ORIENTED_EDGE ( 'NONE', *, *, #2639, .F. ) ;
#408 = CARTESIAN_POINT ( 'NONE',  ( -16.29350689640809691, -140.1746510883711778, -27.01918567566963247 ) ) ;
#409 =( GEOMETRIC_REPRESENTATION_CONTEXT ( 3 ) GLOBAL_UNCERTAINTY_ASSIGNED_CONTEXT ( ( #7381 ) ) GLOBAL_UNIT_ASSIGNED_CONTEXT ( ( #5955, #7452, #1930 ) ) REPRESENTATION_CONTEXT ( 'NONE', 'WORKASPACE' ) );
#410 = EDGE_LOOP ( 'NONE', ( #1681, #5239, #2854, #5762 ) ) ;
#411 =( LENGTH_UNIT ( ) NAMED_UNIT ( * ) SI_UNIT ( .MILLI., .METRE. ) );
#412 = EDGE_LOOP ( 'NONE', ( #6955, #1615, #901, #8803 ) ) ;
#413 = CARTESIAN_POINT ( 'NONE',  ( 39.99999999999997158, -145.1457019118819005, 43.99999999999997158 ) ) ;
#414 = EDGE_CURVE ( 'NONE', #7304, #3508, #5358, .T. ) ;
#415 = VERTEX_POINT ( 'NONE', #7799 ) ;
#416 = AXIS2_PLACEMENT_3D ( 'NONE', #6605, #8136, #2577 ) ;
#417 = EDGE_LOOP ( 'NONE', ( #9129, #8293, #8027, #4721 ) ) ;
#418 = CARTESIAN_POINT ( 'NONE',  ( -7.293506896408097795, 4.007378841484243628E-15, -28.00000000000002132 ) ) ;
#419 = ORIENTED_EDGE ( 'NONE', *, *, #2627, .T. ) ;
#420 = SURFACE_STYLE_USAGE ( .BOTH. , #5282 ) ;
#421 = FACE_OUTER_BOUND ( 'NONE', #4486, .T. ) ;
#422 = DIRECTION ( 'NONE',  ( -1.000000000000000000, -0.000000000000000000, -0.000000000000000000 ) ) ;
#423 = LINE ( 'NONE', #8528, #19 ) ;
#424 = VECTOR ( 'NONE', #10366, 1000.000000000000000 ) ;
#425 = ORIENTED_EDGE ( 'NONE', *, *, #4709, .F. ) ;
#426 = VERTEX_POINT ( 'NONE', #6154 ) ;
#427 = CARTESIAN_POINT ( 'NONE',  ( 39.99999999999998579, -135.1457019118818721, -40.00000000000002132 ) ) ;
#428 = EDGE_CURVE ( 'NONE', #3827, #4373, #811, .T. ) ;
#429 = EDGE_CURVE ( 'NONE', #10221, #9616, #9343, .T. ) ;
#430 = EDGE_CURVE ( 'NONE', #1386, #2425, #494, .T. ) ;
#431 = ORIENTED_EDGE ( 'NONE', *, *, #8121, .T. ) ;
#432 = DIRECTION ( 'NONE',  ( 1.000000000000000000, -0.000000000000000000, -0.000000000000000000 ) ) ;
#433 = DIRECTION ( 'NONE',  ( 0.000000000000000000, 0.000000000000000000, 1.000000000000000000 ) ) ;
#434 = VECTOR ( 'NONE', #2697, 1000.000000000000000 ) ;
#435 = CARTESIAN_POINT ( 'NONE',  ( -20.29350689640809691, 140.5696653505793563, -7.749999999999996447 ) ) ;
#436 = CARTESIAN_POINT ( 'NONE',  ( 39.99999999999998579, -135.1457019118818721, -44.02500000000001990 ) ) ;
#437 = CIRCLE ( 'NONE', #6179, 10.00000000000000178 ) ;
#438 = ORIENTED_EDGE ( 'NONE', *, *, #7577, .T. ) ;
#439 = ORIENTED_EDGE ( 'NONE', *, *, #3690, .T. ) ;
#440 = ORIENTED_EDGE ( 'NONE', *, *, #2696, .F. ) ;
#441 = EDGE_CURVE ( 'NONE', #6928, #4613, #975, .T. ) ;
#442 = EDGE_LOOP ( 'NONE', ( #9473, #3806 ) ) ;
#443 = ORIENTED_EDGE ( 'NONE', *, *, #6054, .F. ) ;
#444 = DIRECTION ( 'NONE',  ( 1.000000000000000000, 0.000000000000000000, 0.000000000000000000 ) ) ;
#445 = FACE_OUTER_BOUND ( 'NONE', #4657, .T. ) ;
#446 = CYLINDRICAL_SURFACE ( 'NONE', #9247, 1.999999999999998224 ) ;
#447 = FACE_OUTER_BOUND ( 'NONE', #1757, .T. ) ;
#448 = FACE_OUTER_BOUND ( 'NONE', #668, .T. ) ;
#449 = AXIS2_PLACEMENT_3D ( 'NONE', #1185, #3570, #1133 ) ;
#450 = ORIENTED_EDGE ( 'NONE', *, *, #5738, .F. ) ;
#451 = DIRECTION ( 'NONE',  ( 1.000000000000000000, 0.000000000000000000, -0.000000000000000000 ) ) ;
#452 = VECTOR ( 'NONE', #3941, 1000.000000000000000 ) ;
#453 = DIRECTION ( 'NONE',  ( 8.379529552680108569E-16, 0.000000000000000000, -1.000000000000000000 ) ) ;
#454 = ORIENTED_EDGE ( 'NONE', *, *, #516, .F. ) ;
#455 = CARTESIAN_POINT ( 'NONE',  ( -8.793506896408096907, 120.5289575273812233, 7.750000000000000000 ) ) ;
#456 = CARTESIAN_POINT ( 'NONE',  ( 23.15769640663935292, -117.1457019118819005, 2.263923683133336310E-14 ) ) ;
#457 = EDGE_CURVE ( 'NONE', #10082, #9303, #1997, .T. ) ;
#458 = DIRECTION ( 'NONE',  ( 0.000000000000000000, 0.000000000000000000, 1.000000000000000000 ) ) ;
#459 = VECTOR ( 'NONE', #2787, 1000.000000000000000 ) ;
#460 = CARTESIAN_POINT ( 'NONE',  ( -40.99999999999999289, -3.464101615137750834, -2.000000000000019096 ) ) ;
#461 = ORIENTED_EDGE ( 'NONE', *, *, #1064, .F. ) ;
#462 = CARTESIAN_POINT ( 'NONE',  ( 0.000000000000000000, -135.1457019118818721, -30.00000000000000355 ) ) ;
#463 = AXIS2_PLACEMENT_3D ( 'NONE', #984, #7454, #8830 ) ;
#464 = ORIENTED_EDGE ( 'NONE', *, *, #46, .F. ) ;
#465 = CARTESIAN_POINT ( 'NONE',  ( -23.15769640663937423, -117.1457019118819005, -50.00000000000002132 ) ) ;
#466 = ORIENTED_EDGE ( 'NONE', *, *, #354, .T. ) ;
#467 = VECTOR ( 'NONE', #4578, 1000.000000000000114 ) ;
#468 = ORIENTED_EDGE ( 'NONE', *, *, #2360, .F. ) ;
#469 = DIRECTION ( 'NONE',  ( 1.000000000000000000, 0.000000000000000000, 0.000000000000000000 ) ) ;
#470 = CARTESIAN_POINT ( 'NONE',  ( 39.99999999999997158, -135.1457019118818721, 39.99999999999997868 ) ) ;
#471 =( NAMED_UNIT ( * ) PLANE_ANGLE_UNIT ( ) SI_UNIT ( $, .RADIAN. ) );
#472 = CARTESIAN_POINT ( 'NONE',  ( 3.000000000000000000, 0.000000000000000000, 0.000000000000000000 ) ) ;
#473 = DIRECTION ( 'NONE',  ( -0.000000000000000000, -1.000000000000000000, -0.000000000000000000 ) ) ;
#474 = FACE_OUTER_BOUND ( 'NONE', #5248, .T. ) ;
#475 = EDGE_CURVE ( 'NONE', #3710, #4318, #8599, .T. ) ;
#476 = VECTOR ( 'NONE', #3446, 1000.000000000000000 ) ;
#477 = VERTEX_POINT ( 'NONE', #4411 ) ;
#478 = CARTESIAN_POINT ( 'NONE',  ( -2.293506896408094242, 152.5696653505793279, -12.50000000000000000 ) ) ;
#479 = EDGE_LOOP ( 'NONE', ( #9318, #5776 ) ) ;
#480 = CARTESIAN_POINT ( 'NONE',  ( 14.70649310359190309, 120.5696653505793705, 20.00000000000000711 ) ) ;
#481 = LINE ( 'NONE', #8373, #6459 ) ;
#482 = CARTESIAN_POINT ( 'NONE',  ( 38.19229777560031636, 118.3760186273086816, -12.50000000000000000 ) ) ;
#483 = CARTESIAN_POINT ( 'NONE',  ( 0.000000000000000000, -115.1457019118818863, -50.00000000000002132 ) ) ;
#484 = DIRECTION ( 'NONE',  ( 0.000000000000000000, -1.000000000000000000, 1.222897680782651471E-16 ) ) ;
#485 = AXIS2_PLACEMENT_3D ( 'NONE', #1777, #6653, #7502 ) ;
#486 = ORIENTED_EDGE ( 'NONE', *, *, #169, .T. ) ;
#487 = ADVANCED_FACE ( 'NONE', ( #1284 ), #6851, .T. ) ;
#488 = ADVANCED_FACE ( 'NONE', ( #4569, #3620 ), #8489, .T. ) ;
#489 = ADVANCED_FACE ( 'NONE', ( #10089 ), #9183, .T. ) ;
#490 = VERTEX_POINT ( 'NONE', #341 ) ;
#491 = VECTOR ( 'NONE', #5813, 1000.000000000000000 ) ;
#492 = ORIENTED_EDGE ( 'NONE', *, *, #6447, .F. ) ;
#493 = VERTEX_POINT ( 'NONE', #2817 ) ;
#494 = LINE ( 'NONE', #10247, #6224 ) ;
#495 = DIRECTION ( 'NONE',  ( 0.000000000000000000, -1.000000000000000000, -1.222897680782651224E-16 ) ) ;
#496 = DIRECTION ( 'NONE',  ( 0.000000000000000000, 1.000000000000000000, 0.000000000000000000 ) ) ;
#497 = CARTESIAN_POINT ( 'NONE',  ( -166.0794662972351716, 270.8019239353934040, 0.000000000000000000 ) ) ;
#498 = PRODUCT_RELATED_PRODUCT_CATEGORY ( 'part', '', ( #2307 ) ) ;
#499 = LINE ( 'NONE', #10311, #7721 ) ;
#500 = EDGE_CURVE ( 'NONE', #47, #3843, #7698, .T. ) ;
#501 = ORIENTED_EDGE ( 'NONE', *, *, #3328, .F. ) ;
#502 = AXIS2_PLACEMENT_3D ( 'NONE', #2591, #6613, #4182 ) ;
#503 = CARTESIAN_POINT ( 'NONE',  ( -117.0000000000000000, -3.592756407884938330, -1.758437202063728666 ) ) ;
#504 = DIRECTION ( 'NONE',  ( 1.000000000000000000, 0.000000000000000000, 0.000000000000000000 ) ) ;
#505 = CARTESIAN_POINT ( 'NONE',  ( 25.15769640663936002, -115.1457019118818863, -3.513494341946486113E-15 ) ) ;
#506 = AXIS2_PLACEMENT_3D ( 'NONE', #5972, #369, #2849 ) ;
#507 = DIRECTION ( 'NONE',  ( -1.000000000000000000, 0.000000000000000000, 0.000000000000000000 ) ) ;
#508 = DIRECTION ( 'NONE',  ( -0.000000000000000000, 1.000000000000000000, -0.000000000000000000 ) ) ;
#509 = FACE_OUTER_BOUND ( 'NONE', #4315, .T. ) ;
#510 = VERTEX_POINT ( 'NONE', #5251 ) ;
#511 = CYLINDRICAL_SURFACE ( 'NONE', #5792, 4.999999999999997335 ) ;
#512 = ORIENTED_EDGE ( 'NONE', *, *, #1198, .F. ) ;
#513 = EDGE_LOOP ( 'NONE', ( #4202, #3563, #1283, #1400 ) ) ;
#514 = LINE ( 'NONE', #8516, #2322 ) ;
#515 = ORIENTED_EDGE ( 'NONE', *, *, #6735, .T. ) ;
#516 = EDGE_CURVE ( 'NONE', #9939, #3381, #7904, .T. ) ;
#517 = EDGE_LOOP ( 'NONE', ( #2540, #3585, #6858, #7797 ) ) ;
#518 = DIRECTION ( 'NONE',  ( -0.000000000000000000, 0.000000000000000000, -1.000000000000000000 ) ) ;
#519 = CARTESIAN_POINT ( 'NONE',  ( 0.000000000000000000, -1.467624384280024730, 2.542000000000003368 ) ) ;
#520 =( LENGTH_UNIT ( ) NAMED_UNIT ( * ) SI_UNIT ( .MILLI., .METRE. ) );
#521 = DIRECTION ( 'NONE',  ( 0.000000000000000000, -1.000000000000000000, 0.000000000000000000 ) ) ;
#522 = DIRECTION ( 'NONE',  ( -1.000000000000000000, -0.000000000000000000, -0.000000000000000000 ) ) ;
#523 = DIRECTION ( 'NONE',  ( 0.000000000000000000, 1.000000000000000000, -0.000000000000000000 ) ) ;
#524 = CARTESIAN_POINT ( 'NONE',  ( -30.29350689640809335, 140.5696653505793563, -20.00000000000000355 ) ) ;
#525 = EDGE_LOOP ( 'NONE', ( #1415, #3468, #7826, #6122 ) ) ;
#526 = PLANE ( 'NONE',  #8406 ) ;
#527 = AXIS2_PLACEMENT_3D ( 'NONE', #7457, #1037, #6552 ) ;
#528 = ORIENTED_EDGE ( 'NONE', *, *, #8703, .F. ) ;
#529 = ADVANCED_FACE ( 'NONE', ( #748 ), #598, .F. ) ;
#530 = DIRECTION ( 'NONE',  ( -1.387778780781445676E-16, 0.000000000000000000, 1.000000000000000000 ) ) ;
#531 = CARTESIAN_POINT ( 'NONE',  ( -2.293506896408097795, 152.5696653505793279, 30.00000000000000355 ) ) ;
#532 = FACE_OUTER_BOUND ( 'NONE', #2911, .T. ) ;
#533 = LINE ( 'NONE', #2178, #8761 ) ;
#534 = DIRECTION ( 'NONE',  ( -1.000000000000000000, 0.000000000000000000, 0.000000000000000000 ) ) ;
#535 = VECTOR ( 'NONE', #5204, 1000.000000000000227 ) ;
#536 = ORIENTED_EDGE ( 'NONE', *, *, #7617, .T. ) ;
#537 = ORIENTED_EDGE ( 'NONE', *, *, #5206, .F. ) ;
#538 = AXIS2_PLACEMENT_3D ( 'NONE', #3174, #3070, #8843 ) ;
#539 = ORIENTED_EDGE ( 'NONE', *, *, #7426, .F. ) ;
#540 = AXIS2_PLACEMENT_3D ( 'NONE', #9014, #1857, #5669 ) ;
#541 = VERTEX_POINT ( 'NONE', #3185 ) ;
#542 = EDGE_CURVE ( 'NONE', #1314, #8114, #798, .T. ) ;
#543 = DIRECTION ( 'NONE',  ( 0.000000000000000000, 0.000000000000000000, -1.000000000000000000 ) ) ;
#544 = CARTESIAN_POINT ( 'NONE',  ( -30.29350689640809335, 37.08684478514406635, -15.00000000000000355 ) ) ;
#545 = ADVANCED_FACE ( 'NONE', ( #7912, #2343, #6211, #4819, #2293 ), #3832, .F. ) ;
#546 = FACE_OUTER_BOUND ( 'NONE', #2266, .T. ) ;
#547 = DIRECTION ( 'NONE',  ( -0.000000000000000000, 1.000000000000000000, -0.000000000000000000 ) ) ;
#548 = DIRECTION ( 'NONE',  ( 0.000000000000000000, -0.000000000000000000, -1.000000000000000000 ) ) ;
#549 = AXIS2_PLACEMENT_3D ( 'NONE', #9186, #9892, #1766 ) ;
#550 = ORIENTED_EDGE ( 'NONE', *, *, #3594, .F. ) ;
#551 = TOROIDAL_SURFACE ( 'NONE', #6465, 16.62298474266377468, 9.050254677131421843 ) ;
#552 = CARTESIAN_POINT ( 'NONE',  ( -48.00000000000002132, -117.1457019118819005, -25.15769640663945950 ) ) ;
#553 = DIRECTION ( 'NONE',  ( 1.000000000000000000, 0.000000000000000000, 0.000000000000000000 ) ) ;
#554 = EDGE_CURVE ( 'NONE', #10372, #47, #7122, .T. ) ;
#555 = ORIENTED_EDGE ( 'NONE', *, *, #457, .T. ) ;
#556 = EDGE_CURVE ( 'NONE', #9911, #2425, #6732, .T. ) ;
#557 = CIRCLE ( 'NONE', #1228, 2.000000000000001776 ) ;
#558 = ADVANCED_FACE ( 'NONE', ( #9507 ), #6568, .T. ) ;
#559 = FACE_OUTER_BOUND ( 'NONE', #2056, .T. ) ;
#560 = CARTESIAN_POINT ( 'NONE',  ( 25.93999053166053415, -135.0799163051958942, -50.00000000000002132 ) ) ;
#561 = CARTESIAN_POINT ( 'NONE',  ( -50.00000000000001421, -145.1457019118819005, -40.00000000000002132 ) ) ;
#562 = ORIENTED_EDGE ( 'NONE', *, *, #7593, .F. ) ;
#563 = DIRECTION ( 'NONE',  ( -1.000000000000000000, 0.000000000000000000, 0.000000000000000000 ) ) ;
#564 = AXIS2_PLACEMENT_3D ( 'NONE', #9552, #1379, #738 ) ;
#565 = EDGE_LOOP ( 'NONE', ( #3764, #4781, #1122, #8407, #4538 ) ) ;
#566 = SHAPE_DEFINITION_REPRESENTATION ( #3920, #9697 ) ;
#567 = ORIENTED_EDGE ( 'NONE', *, *, #7866, .T. ) ;
#568 = CARTESIAN_POINT ( 'NONE',  ( -40.00000000000002842, -135.1457019118818721, 39.99999999999997868 ) ) ;
#569 = ORIENTED_EDGE ( 'NONE', *, *, #2486, .T. ) ;
#570 = ADVANCED_FACE ( 'NONE', ( #6415 ), #698, .F. ) ;
#571 = ORIENTED_EDGE ( 'NONE', *, *, #1163, .T. ) ;
#572 = DIRECTION ( 'NONE',  ( -1.000000000000000000, 0.000000000000000000, 0.000000000000000000 ) ) ;
#573 = DIRECTION ( 'NONE',  ( 0.000000000000000000, 1.000000000000000000, 0.000000000000000000 ) ) ;
#574 = AXIS2_PLACEMENT_3D ( 'NONE', #10123, #6882, #3549 ) ;
#575 = LINE ( 'NONE', #9043, #126 ) ;
#576 = CARTESIAN_POINT ( 'NONE',  ( -89.14744694221916177, 254.1708682956268603, 0.000000000000000000 ) ) ;
#577 = VECTOR ( 'NONE', #1492, 1000.000000000000000 ) ;
#578 = FACE_BOUND ( 'NONE', #834, .T. ) ;
#579 = CARTESIAN_POINT ( 'NONE',  ( -20.29350689640809691, 140.5696653505793563, -20.00000000000000355 ) ) ;
#580 = ADVANCED_FACE ( 'NONE', ( #5467, #8756 ), #7961, .F. ) ;
#581 = VERTEX_POINT ( 'NONE', #8700 ) ;
#582 = CIRCLE ( 'NONE', #8191, 5.000000000000000888 ) ;
#583 = DIRECTION ( 'NONE',  ( 0.000000000000000000, 0.000000000000000000, -1.000000000000000000 ) ) ;
#584 = AXIS2_PLACEMENT_3D ( 'NONE', #2205, #7035, #670 ) ;
#585 = ORIENTED_EDGE ( 'NONE', *, *, #5654, .F. ) ;
#586 = CARTESIAN_POINT ( 'NONE',  ( -48.00000000000002132, -117.1457019118819005, -23.15769640663945594 ) ) ;
#587 = DIRECTION ( 'NONE',  ( -0.000000000000000000, 0.000000000000000000, -1.000000000000000000 ) ) ;
#588 = CARTESIAN_POINT ( 'NONE',  ( 26.00000000000000355, 0.000000000000000000, 2.445500000000000007 ) ) ;
#589 = CARTESIAN_POINT ( 'NONE',  ( 14.70649310359190309, 120.5696653505793705, -20.00000000000000711 ) ) ;
#590 = AXIS2_PLACEMENT_3D ( 'NONE', #6539, #4054, #8179 ) ;
#591 = DIRECTION ( 'NONE',  ( 0.000000000000000000, -1.000000000000000000, -9.100899318238089922E-17 ) ) ;
#592 = ORIENTED_EDGE ( 'NONE', *, *, #303, .F. ) ;
#593 = ORIENTED_EDGE ( 'NONE', *, *, #10466, .T. ) ;
#594 = AXIS2_PLACEMENT_3D ( 'NONE', #3166, #9596, #3115 ) ;
#595 = CIRCLE ( 'NONE', #4810, 2.000000000000001776 ) ;
#596 = VERTEX_POINT ( 'NONE', #7217 ) ;
#597 = ORIENTED_EDGE ( 'NONE', *, *, #4012, .F. ) ;
#598 = PLANE ( 'NONE',  #1493 ) ;
#599 = CARTESIAN_POINT ( 'NONE',  ( 42.22511195853869026, -135.1457019118818721, -25.00000000000000355 ) ) ;
#600 = CARTESIAN_POINT ( 'NONE',  ( 26.00000000000000355, 0.000000000000000000, 0.000000000000000000 ) ) ;
#601 = CARTESIAN_POINT ( 'NONE',  ( -47.94539818030328604, 70.52895752738115220, 0.000000000000000000 ) ) ;
#602 = DIRECTION ( 'NONE',  ( -0.000000000000000000, 1.000000000000000000, -0.000000000000000000 ) ) ;
#603 = ORIENTED_EDGE ( 'NONE', *, *, #3823, .F. ) ;
#604 = DIRECTION ( 'NONE',  ( 0.000000000000000000, 0.000000000000000000, 1.000000000000000000 ) ) ;
#605 = ADVANCED_FACE ( 'NONE', ( #5619 ), #1444, .F. ) ;
#606 = VECTOR ( 'NONE', #7199, 1000.000000000000000 ) ;
#607 = ORIENTED_EDGE ( 'NONE', *, *, #10176, .F. ) ;
#608 = DIRECTION ( 'NONE',  ( 1.000000000000000000, -1.000802005371234881E-16, 6.116012255046435111E-17 ) ) ;
#609 = AXIS2_PLACEMENT_3D ( 'NONE', #4481, #3581, #5958 ) ;
#610 = DIRECTION ( 'NONE',  ( 0.000000000000000000, 1.000000000000000000, 0.000000000000000000 ) ) ;
#611 = CARTESIAN_POINT ( 'NONE',  ( 25.28853996896956247, -134.8487302617674857, -50.00000000000001421 ) ) ;
#612 = DIRECTION ( 'NONE',  ( 1.000000000000000000, 0.000000000000000000, 1.387778780781445676E-16 ) ) ;
#613 = ORIENTED_EDGE ( 'NONE', *, *, #690, .T. ) ;
#614 = CARTESIAN_POINT ( 'NONE',  ( -47.94539818030330025, 150.5696653505793563, 4.025000000000000355 ) ) ;
#615 = EDGE_CURVE ( 'NONE', #2082, #4136, #3892, .T. ) ;
#616 = ADVANCED_FACE ( 'NONE', ( #8805 ), #1548, .T. ) ;
#617 = CIRCLE ( 'NONE', #1964, 4.295524112943372330 ) ;
#618 = EDGE_CURVE ( 'NONE', #5017, #8294, #9061, .T. ) ;
#619 = ORIENTED_EDGE ( 'NONE', *, *, #4744, .F. ) ;
#620 = CIRCLE ( 'NONE', #8401, 2.000000000000001776 ) ;
#621 = CARTESIAN_POINT ( 'NONE',  ( -30.29350689640809335, 145.5696653505793563, 20.00000000000000711 ) ) ;
#622 = ORIENTED_EDGE ( 'NONE', *, *, #3207, .F. ) ;
#623 = VERTEX_POINT ( 'NONE', #3349 ) ;
#624 = DIRECTION ( 'NONE',  ( 0.000000000000000000, 0.000000000000000000, 1.000000000000000000 ) ) ;
#625 = DIRECTION ( 'NONE',  ( 0.000000000000000000, 0.000000000000000000, -1.000000000000000000 ) ) ;
#626 = CIRCLE ( 'NONE', #3497, 2.000000000000001776 ) ;
#627 = DIRECTION ( 'NONE',  ( -0.000000000000000000, 1.000000000000000000, -0.000000000000000000 ) ) ;
#628 = CARTESIAN_POINT ( 'NONE',  ( 39.99999999999998579, -135.1457019118818721, -40.00000000000002132 ) ) ;
#629 = DIRECTION ( 'NONE',  ( -0.000000000000000000, 1.000000000000000000, -0.000000000000000000 ) ) ;
#630 = AXIS2_PLACEMENT_3D ( 'NONE', #7481, #3400, #1118 ) ;
#631 = PLANE ( 'NONE',  #5090 ) ;
#632 = AXIS2_PLACEMENT_3D ( 'NONE', #2833, #3634, #7710 ) ;
#633 = DIRECTION ( 'NONE',  ( 0.000000000000000000, -1.000000000000000000, 0.000000000000000000 ) ) ;
#634 = EDGE_CURVE ( 'NONE', #2019, #13, #4708, .T. ) ;
#635 = ORIENTED_EDGE ( 'NONE', *, *, #3138, .T. ) ;
#636 = VECTOR ( 'NONE', #2330, 1000.000000000000000 ) ;
#637 = CARTESIAN_POINT ( 'NONE',  ( 4.856471286862175774, 152.5696653505793279, -25.00000000000000355 ) ) ;
#638 = ADVANCED_BREP_SHAPE_REPRESENTATION ( '', ( #3440, #4601 ), #9171 ) ;
#639 = VECTOR ( 'NONE', #7530, 1000.000000000000000 ) ;
#640 = VERTEX_POINT ( 'NONE', #4082 ) ;
#641 = CARTESIAN_POINT ( 'NONE',  ( -16.29350689640809691, -140.1746510883711778, 0.000000000000000000 ) ) ;
#642 = DIRECTION ( 'NONE',  ( 0.000000000000000000, -0.000000000000000000, -1.000000000000000000 ) ) ;
#643 = FACE_OUTER_BOUND ( 'NONE', #4818, .T. ) ;
#644 = FACE_OUTER_BOUND ( 'NONE', #7569, .T. ) ;
#645 = CIRCLE ( 'NONE', #4022, 2.000000000000001776 ) ;
#646 = APPLICATION_CONTEXT ( 'automotive_design' ) ;
#647 = FACE_OUTER_BOUND ( 'NONE', #2117, .T. ) ;
#648 = ORIENTED_EDGE ( 'NONE', *, *, #9261, .F. ) ;
#649 = ORIENTED_EDGE ( 'NONE', *, *, #8829, .F. ) ;
#650 = CIRCLE ( 'NONE', #9099, 5.000000000000000888 ) ;
#651 = AXIS2_PLACEMENT_3D ( 'NONE', #10194, #3565, #8546 ) ;
#652 = ORIENTED_EDGE ( 'NONE', *, *, #2869, .T. ) ;
#653 = ORIENTED_EDGE ( 'NONE', *, *, #2945, .T. ) ;
#654 = CARTESIAN_POINT ( 'NONE',  ( 0.3000000000000016542, 0.000000000000000000, 0.000000000000000000 ) ) ;
#655 = EDGE_CURVE ( 'NONE', #2542, #4089, #1011, .T. ) ;
#656 = PLANE ( 'NONE',  #8662 ) ;
#657 = CARTESIAN_POINT ( 'NONE',  ( -7.293506896408097795, 4.007378841484243628E-15, 28.00000000000002132 ) ) ;
#658 = CARTESIAN_POINT ( 'NONE',  ( -7.293506896408097795, 80.56966535057935630, -20.00000000000000711 ) ) ;
#659 = DIRECTION ( 'NONE',  ( 0.000000000000000000, 0.000000000000000000, -1.000000000000000000 ) ) ;
#660 = CIRCLE ( 'NONE', #4540, 4.000000000000000000 ) ;
#661 = ORIENTED_EDGE ( 'NONE', *, *, #1974, .F. ) ;
#662 = DIRECTION ( 'NONE',  ( 1.000000000000000000, 0.000000000000000000, 0.000000000000000000 ) ) ;
#663 = ORIENTED_EDGE ( 'NONE', *, *, #7153, .F. ) ;
#664 = EDGE_CURVE ( 'NONE', #954, #4361, #955, .T. ) ;
#665 = LINE ( 'NONE', #3847, #1646 ) ;
#666 = CARTESIAN_POINT ( 'NONE',  ( 39.99999999999998579, -145.1457019118819005, -36.00000000000002842 ) ) ;
#667 = DIRECTION ( 'NONE',  ( 0.000000000000000000, 0.000000000000000000, 1.000000000000000000 ) ) ;
#668 = EDGE_LOOP ( 'NONE', ( #1329, #7723 ) ) ;
#669 = CARTESIAN_POINT ( 'NONE',  ( -16.29350689640809691, -186.9457019118818835, 0.000000000000000000 ) ) ;
#670 = DIRECTION ( 'NONE',  ( 1.000000000000000000, 0.000000000000000000, 0.000000000000000000 ) ) ;
#671 = ORIENTED_EDGE ( 'NONE', *, *, #4878, .T. ) ;
#672 = DIRECTION ( 'NONE',  ( 0.000000000000000000, 0.5735764363510477137, -0.8191520442889906883 ) ) ;
#673 = CIRCLE ( 'NONE', #7114, 0.2999999999999999334 ) ;
#674 = ORIENTED_EDGE ( 'NONE', *, *, #2905, .T. ) ;
#675 = EDGE_LOOP ( 'NONE', ( #1333, #9999, #2381, #686 ) ) ;
#676 = ADVANCED_FACE ( 'NONE', ( #10, #4242 ), #5668, .F. ) ;
#677 = EDGE_CURVE ( 'NONE', #4096, #6235, #1697, .T. ) ;
#678 = EDGE_CURVE ( 'NONE', #9023, #6043, #1805, .T. ) ;
#679 = CYLINDRICAL_SURFACE ( 'NONE', #6216, 5.000000000000000000 ) ;
#680 = CARTESIAN_POINT ( 'NONE',  ( -166.0794662972351716, 270.8019239353934040, 0.000000000000000000 ) ) ;
#681 = FACE_OUTER_BOUND ( 'NONE', #5766, .T. ) ;
#682 = CARTESIAN_POINT ( 'NONE',  ( -47.94539818030328604, 70.52895752738115220, -4.000000000000000000 ) ) ;
#683 = DIRECTION ( 'NONE',  ( 0.000000000000000000, 0.000000000000000000, 1.000000000000000000 ) ) ;
#684 = EDGE_LOOP ( 'NONE', ( #10046, #2690, #7813, #7655 ) ) ;
#685 = DIRECTION ( 'NONE',  ( 1.000000000000000000, 0.000000000000000000, 0.000000000000000000 ) ) ;
#686 = ORIENTED_EDGE ( 'NONE', *, *, #10087, .F. ) ;
#687 = PRODUCT_DEFINITION ( 'UNKNOWN', '', #247, #5891 ) ;
#688 = CARTESIAN_POINT ( 'NONE',  ( -25.15769640663940976, -133.1457019118818721, 47.99999999999997868 ) ) ;
#689 = CARTESIAN_POINT ( 'NONE',  ( -117.0000000000000000, 3.592756407884963643, -1.758437202063677596 ) ) ;
#690 = EDGE_CURVE ( 'NONE', #1644, #4219, #1648, .T. ) ;
#691 = EDGE_CURVE ( 'NONE', #1746, #382, #7319, .T. ) ;
#692 = FACE_OUTER_BOUND ( 'NONE', #7714, .T. ) ;
#693 = PLANE ( 'NONE',  #3300 ) ;
#694 = DIRECTION ( 'NONE',  ( 0.000000000000000000, -1.000000000000000000, 0.000000000000000000 ) ) ;
#695 = ORIENTED_EDGE ( 'NONE', *, *, #3251, .F. ) ;
#696 = EDGE_LOOP ( 'NONE', ( #7582, #6873 ) ) ;
#697 = EDGE_LOOP ( 'NONE', ( #5887, #6931, #9069, #397 ) ) ;
#698 = CYLINDRICAL_SURFACE ( 'NONE', #3691, 3.297986701801175258 ) ;
#699 = CARTESIAN_POINT ( 'NONE',  ( -36.36957570605426326, 137.0132282531173473, 4.000000000000003553 ) ) ;
#700 = AXIS2_PLACEMENT_3D ( 'NONE', #4653, #4706, #8680 ) ;
#701 = LINE ( 'NONE', #5621, #2314 ) ;
#702 = DIRECTION ( 'NONE',  ( -0.7431448254773957984, 0.6691306063588565722, -0.000000000000000000 ) ) ;
#703 = DIRECTION ( 'NONE',  ( 1.000000000000000000, 0.000000000000000000, 0.000000000000000000 ) ) ;
#704 = ORIENTED_EDGE ( 'NONE', *, *, #31, .F. ) ;
#705 = DIRECTION ( 'NONE',  ( -1.000000000000000000, 0.000000000000000000, 0.000000000000000000 ) ) ;
#706 = ADVANCED_FACE ( 'NONE', ( #4191 ), #8961, .T. ) ;
#707 = CIRCLE ( 'NONE', #1387, 19.24539146688411506 ) ;
#708 = VECTOR ( 'NONE', #5359, 1000.000000000000000 ) ;
#709 = ORIENTED_EDGE ( 'NONE', *, *, #9893, .T. ) ;
#710 = CARTESIAN_POINT ( 'NONE',  ( 27.15769640663935647, -133.1457019118818721, 2.654968395591742513E-14 ) ) ;
#711 = AXIS2_PLACEMENT_3D ( 'NONE', #4492, #7625, #2051 ) ;
#712 =( REPRESENTATION_RELATIONSHIP ('NONE','NONE', #9007, #5068 ) REPRESENTATION_RELATIONSHIP_WITH_TRANSFORMATION ( #7286 )SHAPE_REPRESENTATION_RELATIONSHIP( ) );
#713 = AXIS2_PLACEMENT_3D ( 'NONE', #6468, #8162, #5720 ) ;
#714 = CARTESIAN_POINT ( 'NONE',  ( 26.62179802177715615, -135.1457019118818721, -50.00000000000002132 ) ) ;
#715 = DIRECTION ( 'NONE',  ( 0.000000000000000000, 0.000000000000000000, -1.000000000000000000 ) ) ;
#716 = VERTEX_POINT ( 'NONE', #2543 ) ;
#717 = CARTESIAN_POINT ( 'NONE',  ( -25.15769640663939199, -133.1457019118818721, -27.15769640663944173 ) ) ;
#718 = APPLICATION_PROTOCOL_DEFINITION ( 'draft international standard', 'automotive_design', 1998, #10047 ) ;
#719 = VERTEX_POINT ( 'NONE', #3233 ) ;
#720 = CIRCLE ( 'NONE', #9019, 4.000000000000000000 ) ;
#721 = LINE ( 'NONE', #3910, #10314 ) ;
#722 = CIRCLE ( 'NONE', #10375, 4.000000000000000000 ) ;
#723 = VERTEX_POINT ( 'NONE', #221 ) ;
#724 = DIRECTION ( 'NONE',  ( 0.000000000000000000, 0.000000000000000000, -1.000000000000000000 ) ) ;
#725 = LINE ( 'NONE', #4650, #5911 ) ;
#726 = DIRECTION ( 'NONE',  ( -0.000000000000000000, 1.000000000000000000, -0.000000000000000000 ) ) ;
#727 = PLANE ( 'NONE',  #5508 ) ;
#728 = TOROIDAL_SURFACE ( 'NONE', #9364, 3.377784142883041074, 6.382478589986769535 ) ;
#729 = CARTESIAN_POINT ( 'NONE',  ( -20.29350689640809691, 140.5696653505793563, 10.90000000000000036 ) ) ;
#730 = DIRECTION ( 'NONE',  ( -9.776117811460147207E-16, 0.000000000000000000, 1.000000000000000000 ) ) ;
#731 = EDGE_CURVE ( 'NONE', #8244, #5058, #3289, .T. ) ;
#732 = VERTEX_POINT ( 'NONE', #2652 ) ;
#733 = CARTESIAN_POINT ( 'NONE',  ( 38.19229777560031636, -43.28483205141633761, 12.50000000000000000 ) ) ;
#734 = CIRCLE ( 'NONE', #7849, 4.000000000000000000 ) ;
#735 = VERTEX_POINT ( 'NONE', #5031 ) ;
#736 = DIRECTION ( 'NONE',  ( 1.000000000000000000, 0.000000000000000000, 0.000000000000000000 ) ) ;
#737 = DIRECTION ( 'NONE',  ( 0.000000000000000000, 0.000000000000000000, 1.000000000000000000 ) ) ;
#738 = DIRECTION ( 'NONE',  ( 0.000000000000000000, -0.000000000000000000, 1.000000000000000000 ) ) ;
#739 = DIRECTION ( 'NONE',  ( 0.000000000000000000, 1.000000000000000000, 0.000000000000000000 ) ) ;
#740 = CARTESIAN_POINT ( 'NONE',  ( -7.293506896408097795, 145.5696653505793563, -25.00000000000000711 ) ) ;
#741 = ORIENTED_EDGE ( 'NONE', *, *, #7129, .T. ) ;
#742 = AXIS2_PLACEMENT_3D ( 'NONE', #6990, #7887, #1423 ) ;
#743 = ORIENTED_EDGE ( 'NONE', *, *, #2625, .F. ) ;
#744 = EDGE_CURVE ( 'NONE', #623, #6132, #1660, .T. ) ;
#745 = EDGE_CURVE ( 'NONE', #2342, #2439, #3018, .T. ) ;
#746 = EDGE_CURVE ( 'NONE', #4432, #1005, #6398, .T. ) ;
#747 = ORIENTED_EDGE ( 'NONE', *, *, #7309, .T. ) ;
#748 = FACE_OUTER_BOUND ( 'NONE', #1862, .T. ) ;
#749 = CARTESIAN_POINT ( 'NONE',  ( -51.88626362769068123, 173.3644333388386940, 4.898587196589412829E-16 ) ) ;
#750 = AXIS2_PLACEMENT_3D ( 'NONE', #8663, #6275, #5427 ) ;
#751 = CARTESIAN_POINT ( 'NONE',  ( 14.70649310359190309, 120.5696653505793705, -24.00000000000000711 ) ) ;
#752 = CARTESIAN_POINT ( 'NONE',  ( 25.15769640663936357, -133.1457019118818721, 27.15769640663938489 ) ) ;
#753 = DIRECTION ( 'NONE',  ( 0.000000000000000000, -0.9374252720097652203, -0.3481865296036273372 ) ) ;
#754 = ORIENTED_EDGE ( 'NONE', *, *, #8274, .T. ) ;
#755 = CARTESIAN_POINT ( 'NONE',  ( -16.29350689640810401, 14.34401513294132613, 0.000000000000000000 ) ) ;
#756 = AXIS2_PLACEMENT_3D ( 'NONE', #4002, #6747, #591 ) ;
#757 = EDGE_CURVE ( 'NONE', #6846, #5066, #8265, .T. ) ;
#758 = ORIENTED_EDGE ( 'NONE', *, *, #3924, .F. ) ;
#759 = CIRCLE ( 'NONE', #7197, 2.541999999999999815 ) ;
#760 = CARTESIAN_POINT ( 'NONE',  ( 23.15769640663936713, -117.1457019118819005, 47.99999999999997868 ) ) ;
#761 = CARTESIAN_POINT ( 'NONE',  ( -7.293506896408097795, 80.56966535057935630, 20.00000000000000711 ) ) ;
#762 = DIRECTION ( 'NONE',  ( -0.000000000000000000, 1.000000000000000000, 0.000000000000000000 ) ) ;
#763 = AXIS2_PLACEMENT_3D ( 'NONE', #4850, #200, #3320 ) ;
#764 = ORIENTED_EDGE ( 'NONE', *, *, #7097, .F. ) ;
#765 = DIRECTION ( 'NONE',  ( -0.6691306063588566833, -0.7431448254773957984, 0.000000000000000000 ) ) ;
#766 = ORIENTED_EDGE ( 'NONE', *, *, #6509, .F. ) ;
#767 = DIRECTION ( 'NONE',  ( -1.000000000000000000, 0.000000000000000000, 0.000000000000000000 ) ) ;
#768 = ORIENTED_EDGE ( 'NONE', *, *, #5611, .F. ) ;
#769 = AXIS2_PLACEMENT_3D ( 'NONE', #8126, #4104, #6540 ) ;
#770 = APPLICATION_CONTEXT ( 'automotive_design' ) ;
#771 = ORIENTED_EDGE ( 'NONE', *, *, #2304, .T. ) ;
#772 = EDGE_CURVE ( 'NONE', #1040, #1722, #2099, .T. ) ;
#773 = FACE_OUTER_BOUND ( 'NONE', #6412, .T. ) ;
#774 = LINE ( 'NONE', #5749, #5140 ) ;
#775 = CARTESIAN_POINT ( 'NONE',  ( -27.15769640663940621, -133.1457019118818721, -3.792811993702496405E-15 ) ) ;
#776 = CIRCLE ( 'NONE', #10093, 10.00000000000000178 ) ;
#777 = LINE ( 'NONE', #4799, #5594 ) ;
#778 = FACE_OUTER_BOUND ( 'NONE', #5546, .T. ) ;
#779 = PRODUCT_DEFINITION_SHAPE ( 'NONE', 'NONE',  #10483 ) ;
#780 = VECTOR ( 'NONE', #9895, 1000.000000000000000 ) ;
#781 = EDGE_LOOP ( 'NONE', ( #592, #10254 ) ) ;
#782 = DIRECTION ( 'NONE',  ( 1.000000000000000000, -0.000000000000000000, -0.000000000000000000 ) ) ;
#783 = VECTOR ( 'NONE', #2800, 999.9999999999998863 ) ;
#784 = ORIENTED_EDGE ( 'NONE', *, *, #5041, .F. ) ;
#785 = CARTESIAN_POINT ( 'NONE',  ( -3.173844575093148990, 90.52895752738122326, -10.90000000000000036 ) ) ;
#786 = DIRECTION ( 'NONE',  ( 0.000000000000000000, 0.000000000000000000, -1.000000000000000000 ) ) ;
#787 = CIRCLE ( 'NONE', #8916, 8.635821936424155965 ) ;
#788 = LINE ( 'NONE', #2, #1240 ) ;
#789 = EDGE_CURVE ( 'NONE', #10120, #2699, #7933, .T. ) ;
#790 = CYLINDRICAL_SURFACE ( 'NONE', #7011, 4.000000000000000000 ) ;
#791 = DIRECTION ( 'NONE',  ( 0.000000000000000000, 0.000000000000000000, -1.000000000000000000 ) ) ;
#792 = ORIENTED_EDGE ( 'NONE', *, *, #6700, .T. ) ;
#793 = CIRCLE ( 'NONE', #2484, 3.999999999999989786 ) ;
#794 = ORIENTED_EDGE ( 'NONE', *, *, #1876, .T. ) ;
#795 = AXIS2_PLACEMENT_3D ( 'NONE', #9143, #5116, #4324 ) ;
#796 = EDGE_LOOP ( 'NONE', ( #3033, #3285, #2044, #4290, #4720, #6254, #6792, #181, #8225, #1496, #6918, #653, #4433, #3564, #275, #5135 ) ) ;
#797 = ORIENTED_EDGE ( 'NONE', *, *, #9578, .T. ) ;
#798 = LINE ( 'NONE', #7169, #6391 ) ;
#799 = CARTESIAN_POINT ( 'NONE',  ( -40.99999999999999289, -5.556536133988210224E-16, 4.000000000000005329 ) ) ;
#800 = AXIS2_PLACEMENT_3D ( 'NONE', #1242, #3197, #6426 ) ;
#801 = DIRECTION ( 'NONE',  ( 0.000000000000000000, -1.000000000000000000, -1.222897680782651471E-16 ) ) ;
#802 = FACE_OUTER_BOUND ( 'NONE', #3369, .T. ) ;
#803 = EDGE_CURVE ( 'NONE', #1658, #1518, #5219, .T. ) ;
#804 = EDGE_CURVE ( 'NONE', #6696, #289, #4348, .T. ) ;
#805 = EDGE_CURVE ( 'NONE', #4824, #2551, #1327, .T. ) ;
#806 = VECTOR ( 'NONE', #507, 1000.000000000000000 ) ;
#807 = ORIENTED_EDGE ( 'NONE', *, *, #5966, .T. ) ;
#808 = DIRECTION ( 'NONE',  ( -1.000000000000000000, 0.000000000000000000, 8.673617379884035472E-17 ) ) ;
#809 = ORIENTED_EDGE ( 'NONE', *, *, #9423, .T. ) ;
#810 = CARTESIAN_POINT ( 'NONE',  ( -142.3328939341254795, 249.4204141414382434, 0.000000000000000000 ) ) ;
#811 = CIRCLE ( 'NONE', #10126, 3.250000000000000444 ) ;
#812 = ORIENTED_EDGE ( 'NONE', *, *, #634, .T. ) ;
#813 = ORIENTED_EDGE ( 'NONE', *, *, #3298, .T. ) ;
#814 = DIRECTION ( 'NONE',  ( 0.000000000000000000, 0.000000000000000000, 1.000000000000000000 ) ) ;
#815 = DIRECTION ( 'NONE',  ( 0.000000000000000000, 0.000000000000000000, -1.000000000000000000 ) ) ;
#816 = VECTOR ( 'NONE', #7358, 1000.000000000000000 ) ;
#817 = EDGE_CURVE ( 'NONE', #4776, #9808, #8534, .T. ) ;
#818 = FACE_OUTER_BOUND ( 'NONE', #3605, .T. ) ;
#819 = CARTESIAN_POINT ( 'NONE',  ( 37.25478555609232245, -134.3993646471907084, -25.57704176894851855 ) ) ;
#820 = ORIENTED_EDGE ( 'NONE', *, *, #10303, .T. ) ;
#821 = LINE ( 'NONE', #4057, #7300 ) ;
#822 = VERTEX_POINT ( 'NONE', #4455 ) ;
#823 = CARTESIAN_POINT ( 'NONE',  ( 4.856471286862173997, 152.5696653505793279, 12.50000000000000000 ) ) ;
#824 = ORIENTED_EDGE ( 'NONE', *, *, #3937, .F. ) ;
#825 = AXIS2_PLACEMENT_3D ( 'NONE', #194, #4265, #2629 ) ;
#826 = VERTEX_POINT ( 'NONE', #2700 ) ;
#827 = DIRECTION ( 'NONE',  ( 0.000000000000000000, 0.000000000000000000, 1.000000000000000000 ) ) ;
#828 = FACE_OUTER_BOUND ( 'NONE', #5278, .T. ) ;
#829 = DIRECTION ( 'NONE',  ( 0.000000000000000000, 0.000000000000000000, -1.000000000000000000 ) ) ;
#830 = FACE_OUTER_BOUND ( 'NONE', #1137, .T. ) ;
#831 = CARTESIAN_POINT ( 'NONE',  ( -37.01000625782472753, 0.000000000000000000, 0.000000000000000000 ) ) ;
#832 = VECTOR ( 'NONE', #8468, 1000.000000000000000 ) ;
#833 = EDGE_CURVE ( 'NONE', #8917, #6087, #10133, .T. ) ;
#834 = EDGE_LOOP ( 'NONE', ( #2251, #3043 ) ) ;
#835 = DIRECTION ( 'NONE',  ( 0.000000000000000000, 0.000000000000000000, 1.000000000000000000 ) ) ;
#836 = VERTEX_POINT ( 'NONE', #2012 ) ;
#837 = CARTESIAN_POINT ( 'NONE',  ( -16.29350689640809691, -186.9457019118818835, -23.72119897386845722 ) ) ;
#838 = DIRECTION ( 'NONE',  ( -1.000000000000000000, 0.000000000000000000, 0.000000000000000000 ) ) ;
#839 = DIRECTION ( 'NONE',  ( -0.000000000000000000, 1.000000000000000000, -0.000000000000000000 ) ) ;
#840 = CARTESIAN_POINT ( 'NONE',  ( -56.36957570605426326, 90.52895752738122326, -10.90000000000000036 ) ) ;
#841 = DIRECTION ( 'NONE',  ( -9.101836848464095537E-17, -0.000000000000000000, -1.000000000000000000 ) ) ;
#842 = DIRECTION ( 'NONE',  ( 0.6585271261848804070, -0.7525569905852197428, 0.000000000000000000 ) ) ;
#843 = ORIENTED_EDGE ( 'NONE', *, *, #5371, .T. ) ;
#844 = ORIENTED_EDGE ( 'NONE', *, *, #4744, .T. ) ;
#845 = ORIENTED_EDGE ( 'NONE', *, *, #1574, .T. ) ;
#846 = EDGE_CURVE ( 'NONE', #10164, #6362, #660, .T. ) ;
#847 = VERTEX_POINT ( 'NONE', #6947 ) ;
#848 = DIRECTION ( 'NONE',  ( 1.000000000000000000, 0.000000000000000000, -0.000000000000000000 ) ) ;
#849 = CARTESIAN_POINT ( 'NONE',  ( -166.0794662972351716, 270.8019239353934040, 0.000000000000000000 ) ) ;
#850 = DIRECTION ( 'NONE',  ( 0.000000000000000000, -1.734723475976808278E-15, 1.000000000000000000 ) ) ;
#851 = DIRECTION ( 'NONE',  ( -0.000000000000000000, -1.000000000000000000, -0.000000000000000000 ) ) ;
#852 = VERTEX_POINT ( 'NONE', #2061 ) ;
#853 = LINE ( 'NONE', #4144, #7394 ) ;
#854 = EDGE_LOOP ( 'NONE', ( #9526, #8200, #20, #9001 ) ) ;
#855 = DIRECTION ( 'NONE',  ( 0.000000000000000000, -0.9374252720097652203, 0.3481865296036273372 ) ) ;
#856 = EDGE_CURVE ( 'NONE', #6933, #6085, #6838, .T. ) ;
#857 = ADVANCED_FACE ( 'NONE', ( #3501 ), #7687, .F. ) ;
#858 = ORIENTED_EDGE ( 'NONE', *, *, #2768, .F. ) ;
#859 = AXIS2_PLACEMENT_3D ( 'NONE', #9746, #8298, #5696 ) ;
#860 = CARTESIAN_POINT ( 'NONE',  ( -20.29350689640809691, 150.5696653505793563, 20.00000000000000355 ) ) ;
#861 = DIRECTION ( 'NONE',  ( 0.000000000000000000, -1.000000000000000000, -1.222897680782651224E-16 ) ) ;
#862 = CARTESIAN_POINT ( 'NONE',  ( 39.99999999999998579, -145.1457019118819005, -50.00000000000002132 ) ) ;
#863 = DIRECTION ( 'NONE',  ( 0.000000000000000000, -1.000000000000000000, 0.000000000000000000 ) ) ;
#864 = AXIS2_PLACEMENT_3D ( 'NONE', #244, #3308, #4941 ) ;
#865 = EDGE_LOOP ( 'NONE', ( #454, #7854, #1982, #1701 ) ) ;
#866=STYLED_ITEM('',(#10532),#9943);
#867 = DIRECTION ( 'NONE',  ( 0.000000000000000000, 0.000000000000000000, 1.000000000000000000 ) ) ;
#868 = EDGE_CURVE ( 'NONE', #10419, #3877, #1219, .T. ) ;
#870 = ADVANCED_FACE ( 'NONE', ( #10077 ), #8372, .T. ) ;
#869 = VERTEX_POINT ( 'NONE', #5345 ) ;
#871 = EDGE_CURVE ( 'NONE', #4076, #4046, #1907, .T. ) ;
#872 = CARTESIAN_POINT ( 'NONE',  ( -26.62179802177716326, -135.1457019118818721, 49.99999999999997868 ) ) ;
#873 = ORIENTED_EDGE ( 'NONE', *, *, #4154, .F. ) ;
#874 = AXIS2_PLACEMENT_3D ( 'NONE', #5517, #1500, #7271 ) ;
#875 = ORIENTED_EDGE ( 'NONE', *, *, #5133, .T. ) ;
#876 = CARTESIAN_POINT ( 'NONE',  ( -23.15769640663940976, -133.1457019118818721, 47.99999999999997868 ) ) ;
#877 = CARTESIAN_POINT ( 'NONE',  ( -20.29350689640809691, 140.5696653505793563, 10.90000000000000036 ) ) ;
#878 = DIRECTION ( 'NONE',  ( 0.000000000000000000, -1.000000000000000000, 0.000000000000000000 ) ) ;
#879 = CARTESIAN_POINT ( 'NONE',  ( -11.29350689640809158, 105.5289575273812233, -10.90000000000000036 ) ) ;
#880 = DIRECTION ( 'NONE',  ( 0.000000000000000000, 1.000000000000000000, 0.000000000000000000 ) ) ;
#881 = CIRCLE ( 'NONE', #385, 4.025000000000000355 ) ;
#882 = CIRCLE ( 'NONE', #9179, 3.999999999999989786 ) ;
#883 = ORIENTED_EDGE ( 'NONE', *, *, #5880, .F. ) ;
#884 = EDGE_CURVE ( 'NONE', #2275, #9529, #6912, .T. ) ;
#885 = CARTESIAN_POINT ( 'NONE',  ( -30.29350689640809335, -0.3998014571812398832, 1.076388538564875708 ) ) ;
#886 = ORIENTED_EDGE ( 'NONE', *, *, #4179, .T. ) ;
#887 = LINE ( 'NONE', #2642, #9640 ) ;
#888 = DIRECTION ( 'NONE',  ( -0.7431448254773957984, 0.6691306063588565722, -0.000000000000000000 ) ) ;
#889 = AXIS2_PLACEMENT_3D ( 'NONE', #4773, #8859, #2296 ) ;
#890 = DIRECTION ( 'NONE',  ( 1.000000000000000000, 0.000000000000000000, 0.000000000000000000 ) ) ;
#891 = CIRCLE ( 'NONE', #3260, 9.050254677131441383 ) ;
#892 = DIRECTION ( 'NONE',  ( -0.7431448254773957984, 0.6691306063588565722, -0.000000000000000000 ) ) ;
#893 = CIRCLE ( 'NONE', #1742, 10.00000000000000178 ) ;
#894 = EDGE_CURVE ( 'NONE', #8252, #3355, #2912, .T. ) ;
#895 = CARTESIAN_POINT ( 'NONE',  ( -40.99999999999999289, 3.464101615137777923, -1.999999999999970468 ) ) ;
#896 = DIRECTION ( 'NONE',  ( 0.000000000000000000, 0.000000000000000000, 1.000000000000000000 ) ) ;
#897 = ORIENTED_EDGE ( 'NONE', *, *, #8642, .F. ) ;
#898 = VERTEX_POINT ( 'NONE', #1955 ) ;
#899 = EDGE_LOOP ( 'NONE', ( #1703, #7682 ) ) ;
#900 = CIRCLE ( 'NONE', #1237, 3.999999999999999112 ) ;
#901 = ORIENTED_EDGE ( 'NONE', *, *, #3298, .F. ) ;
#902 = DIRECTION ( 'NONE',  ( -0.6691306063588566833, -0.7431448254773955764, 0.000000000000000000 ) ) ;
#903 =( NAMED_UNIT ( * ) PLANE_ANGLE_UNIT ( ) SI_UNIT ( $, .RADIAN. ) );
#904 = DIRECTION ( 'NONE',  ( 1.000000000000000000, -0.000000000000000000, -0.000000000000000000 ) ) ;
#905 = EDGE_CURVE ( 'NONE', #7935, #1253, #5191, .T. ) ;
#906 = DIRECTION ( 'NONE',  ( 0.000000000000000000, -1.000000000000000000, 0.000000000000000000 ) ) ;
#907 = VECTOR ( 'NONE', #3811, 1000.000000000000000 ) ;
#908 = ORIENTED_EDGE ( 'NONE', *, *, #1874, .F. ) ;
#909 = CARTESIAN_POINT ( 'NONE',  ( -23.76520584195948516, -145.1457019118819005, 49.99999999999997868 ) ) ;
#910 = VERTEX_POINT ( 'NONE', #2118 ) ;
#911 = DIRECTION ( 'NONE',  ( 0.000000000000000000, 0.000000000000000000, 1.000000000000000000 ) ) ;
#912 = CIRCLE ( 'NONE', #6843, 7.499999999999998224 ) ;
#913 = ORIENTED_EDGE ( 'NONE', *, *, #10013, .T. ) ;
#914 = PRODUCT_DEFINITION_CONTEXT ( 'detailed design', #6791, 'design' ) ;
#915 = LINE ( 'NONE', #4150, #9967 ) ;
#916 = DIRECTION ( 'NONE',  ( -0.7367503238654704578, 0.6761648913424330720, 0.000000000000000000 ) ) ;
#917 = AXIS2_PLACEMENT_3D ( 'NONE', #4642, #9528, #10371 ) ;
#918 = DIRECTION ( 'NONE',  ( -0.000000000000000000, -0.000000000000000000, -1.000000000000000000 ) ) ;
#919 = CARTESIAN_POINT ( 'NONE',  ( 23.15769640663936002, -117.1457019118819005, -3.234176690190481738E-15 ) ) ;
#920 = DIRECTION ( 'NONE',  ( 1.137729606058012035E-16, 0.000000000000000000, 1.000000000000000000 ) ) ;
#921 = ADVANCED_FACE ( 'NONE', ( #8585 ), #1168, .T. ) ;
#922 = DIRECTION ( 'NONE',  ( 0.000000000000000000, 1.000000000000000000, 0.000000000000000000 ) ) ;
#923 = ORIENTED_EDGE ( 'NONE', *, *, #5411, .F. ) ;
#924 = DIRECTION ( 'NONE',  ( 1.000000000000000000, 0.000000000000000000, 0.000000000000000000 ) ) ;
#925 = ORIENTED_EDGE ( 'NONE', *, *, #3802, .T. ) ;
#926 = CYLINDRICAL_SURFACE ( 'NONE', #6588, 2.000000000000001776 ) ;
#927 = ORIENTED_EDGE ( 'NONE', *, *, #103, .F. ) ;
#928 = CIRCLE ( 'NONE', #6857, 2.000000000000001776 ) ;
#929 = ORIENTED_EDGE ( 'NONE', *, *, #6063, .T. ) ;
#930 = AXIS2_PLACEMENT_3D ( 'NONE', #9430, #3015, #2164 ) ;
#931 = CARTESIAN_POINT ( 'NONE',  ( -16.29350689640809691, -19.43033464942062238, 0.000000000000000000 ) ) ;
#932 = CARTESIAN_POINT ( 'NONE',  ( 39.99999999999997158, -135.1707019118818778, 43.99999999999997868 ) ) ;
#933 = EDGE_CURVE ( 'NONE', #1886, #7639, #7594, .T. ) ;
#934 = EDGE_CURVE ( 'NONE', #8880, #7785, #4717, .T. ) ;
#935 = CARTESIAN_POINT ( 'NONE',  ( -20.29350689640809691, 140.5696653505793563, -20.00000000000000711 ) ) ;
#936 = ADVANCED_FACE ( 'NONE', ( #9439 ), #3069, .F. ) ;
#937 = SURFACE_STYLE_FILL_AREA ( #1731 ) ;
#938 = DIRECTION ( 'NONE',  ( 1.000000000000000000, -0.000000000000000000, -0.000000000000000000 ) ) ;
#939 = VERTEX_POINT ( 'NONE', #4556 ) ;
#940 = DIRECTION ( 'NONE',  ( 0.000000000000000000, 0.000000000000000000, 1.000000000000000000 ) ) ;
#941 = VERTEX_POINT ( 'NONE', #3973 ) ;
#942 = DIRECTION ( 'NONE',  ( -1.000000000000000000, -0.000000000000000000, -0.000000000000000000 ) ) ;
#943 = LINE ( 'NONE', #3385, #4422 ) ;
#944 = AXIS2_PLACEMENT_3D ( 'NONE', #7492, #6536, #4207 ) ;
#945 = LINE ( 'NONE', #2479, #10150 ) ;
#946 = DIRECTION ( 'NONE',  ( 0.000000000000000000, -0.9374252720097652203, 0.3481865296036273372 ) ) ;
#947 = CARTESIAN_POINT ( 'NONE',  ( 53.40242741783141156, 52.77167129626698028, 30.00000000000000355 ) ) ;
#948 = VECTOR ( 'NONE', #9800, 1000.000000000000000 ) ;
#949 = ADVANCED_FACE ( 'NONE', ( #5504 ), #7205, .T. ) ;
#950 = CARTESIAN_POINT ( 'NONE',  ( -56.36957570605427748, 150.5696653505793563, -10.90000000000000036 ) ) ;
#951 = ORIENTED_EDGE ( 'NONE', *, *, #10279, .F. ) ;
#952 = ORIENTED_EDGE ( 'NONE', *, *, #17, .F. ) ;
#953 = AXIS2_PLACEMENT_3D ( 'NONE', #5208, #2131, #392 ) ;
#954 = VERTEX_POINT ( 'NONE', #10390 ) ;
#955 = LINE ( 'NONE', #8910, #476 ) ;
#956 = LINE ( 'NONE', #5088, #218 ) ;
#957 = LINE ( 'NONE', #3504, #7581 ) ;
#958 = AXIS2_PLACEMENT_3D ( 'NONE', #8255, #9913, #940 ) ;
#959 = ORIENTED_EDGE ( 'NONE', *, *, #884, .F. ) ;
#960 = CARTESIAN_POINT ( 'NONE',  ( -47.94539818030330025, 150.5446653505793790, -3.999999999999989786 ) ) ;
#961 = AXIS2_PLACEMENT_3D ( 'NONE', #4774, #8012, #3991 ) ;
#962 = ORIENTED_EDGE ( 'NONE', *, *, #8063, .T. ) ;
#963 = AXIS2_PLACEMENT_3D ( 'NONE', #2254, #1408, #9464 ) ;
#964 = EDGE_CURVE ( 'NONE', #1886, #6595, #6232, .T. ) ;
#965 = AXIS2_PLACEMENT_3D ( 'NONE', #710, #3147, #6378 ) ;
#966 = ORIENTED_EDGE ( 'NONE', *, *, #993, .T. ) ;
#967 = EDGE_LOOP ( 'NONE', ( #3889, #1251, #4780, #8395, #6209, #5356, #4672 ) ) ;
#968 = FACE_OUTER_BOUND ( 'NONE', #5774, .T. ) ;
#969 = CARTESIAN_POINT ( 'NONE',  ( 39.99999999999998579, -135.1457019118818721, -40.00000000000002132 ) ) ;
#970 = AXIS2_PLACEMENT_3D ( 'NONE', #4406, #7635, #2757 ) ;
#971 = CYLINDRICAL_SURFACE ( 'NONE', #9240, 2.000000000000001776 ) ;
#972 = DIRECTION ( 'NONE',  ( 1.000000000000000000, 0.000000000000000000, -0.000000000000000000 ) ) ;
#973 = DIRECTION ( 'NONE',  ( 0.000000000000000000, 0.000000000000000000, -1.000000000000000000 ) ) ;
#974 = LINE ( 'NONE', #1562, #1121 ) ;
#975 = CIRCLE ( 'NONE', #7407, 8.000000000000000000 ) ;
#976 = ORIENTED_EDGE ( 'NONE', *, *, #8479, .T. ) ;
#977 = LINE ( 'NONE', #2569, #3578 ) ;
#978 = APPLICATION_PROTOCOL_DEFINITION ( 'draft international standard', 'automotive_design', 1998, #5107 ) ;
#979 = VERTEX_POINT ( 'NONE', #8688 ) ;
#980 = DIRECTION ( 'NONE',  ( -7.016001027857739179E-17, -0.8191520442889906883, -0.5735764363510477137 ) ) ;
#981 = EDGE_CURVE ( 'NONE', #2288, #3945, #9975, .T. ) ;
#982 = ORIENTED_EDGE ( 'NONE', *, *, #7902, .T. ) ;
#983 = AXIS2_PLACEMENT_3D ( 'NONE', #6893, #2860, #6090 ) ;
#984 = CARTESIAN_POINT ( 'NONE',  ( 0.000000000000000000, -115.1457019118818863, 49.99999999999997868 ) ) ;
#985 = AXIS2_PLACEMENT_3D ( 'NONE', #3858, #8781, #7242 ) ;
#986 = FACE_OUTER_BOUND ( 'NONE', #2888, .T. ) ;
#987 = DIRECTION ( 'NONE',  ( 0.000000000000000000, 0.000000000000000000, 1.000000000000000000 ) ) ;
#988 = CARTESIAN_POINT ( 'NONE',  ( -27.15769640663939555, -133.1457019118818721, -27.15769640663944173 ) ) ;
#989 = FACE_OUTER_BOUND ( 'NONE', #8861, .T. ) ;
#990 = AXIS2_PLACEMENT_3D ( 'NONE', #4438, #1044, #2000 ) ;
#991 = VERTEX_POINT ( 'NONE', #7996 ) ;
#992 = DIRECTION ( 'NONE',  ( -1.000000000000000000, 0.000000000000000000, 0.000000000000000000 ) ) ;
#993 = EDGE_CURVE ( 'NONE', #2923, #9336, #1538, .T. ) ;
#994 = EDGE_CURVE ( 'NONE', #9955, #2474, #3183, .T. ) ;
#995 = EDGE_CURVE ( 'NONE', #8447, #1314, #3880, .T. ) ;
#996 = VERTEX_POINT ( 'NONE', #688 ) ;
#997 = CARTESIAN_POINT ( 'NONE',  ( 26.62179802177715615, -135.1457019118818721, -50.00000000000002132 ) ) ;
#998 = DIRECTION ( 'NONE',  ( 6.106226635438360972E-16, -1.000000000000000000, 0.000000000000000000 ) ) ;
#999 = CARTESIAN_POINT ( 'NONE',  ( -25.15769640663939199, -115.1457019118818863, -27.15769640663944173 ) ) ;
#1000 = DIRECTION ( 'NONE',  ( -0.000000000000000000, -0.000000000000000000, -1.000000000000000000 ) ) ;
#1001 = CARTESIAN_POINT ( 'NONE',  ( -40.00000000000002842, -135.1457019118818721, 49.99999999999997868 ) ) ;
#1002 = DIRECTION ( 'NONE',  ( 0.000000000000000000, 1.000000000000000000, 0.000000000000000000 ) ) ;
#1003 =( GEOMETRIC_REPRESENTATION_CONTEXT ( 3 ) GLOBAL_UNCERTAINTY_ASSIGNED_CONTEXT ( ( #1512 ) ) GLOBAL_UNIT_ASSIGNED_CONTEXT ( ( #2813, #9988, #8280 ) ) REPRESENTATION_CONTEXT ( 'NONE', 'WORKASPACE' ) );
#1004 = ORIENTED_EDGE ( 'NONE', *, *, #6311, .T. ) ;
#1005 = VERTEX_POINT ( 'NONE', #3765 ) ;
#1006 = EDGE_CURVE ( 'NONE', #6072, #6663, #8634, .T. ) ;
#1007 = EDGE_CURVE ( 'NONE', #1903, #826, #8841, .T. ) ;
#1008 = ORIENTED_EDGE ( 'NONE', *, *, #7644, .F. ) ;
#1009 = EDGE_CURVE ( 'NONE', #59, #2261, #9804, .T. ) ;
#1010 = AXIS2_PLACEMENT_3D ( 'NONE', #9428, #2213, #2270 ) ;
#1011 = LINE ( 'NONE', #4973, #5882 ) ;
#1012 = LINE ( 'NONE', #7373, #2929 ) ;
#1013 = CARTESIAN_POINT ( 'NONE',  ( 25.15769640663936357, -115.1457019118818863, 27.15769640663938489 ) ) ;
#1014 = ORIENTED_EDGE ( 'NONE', *, *, #5714, .T. ) ;
#1015 = LINE ( 'NONE', #524, #8409 ) ;
#1016 = ORIENTED_EDGE ( 'NONE', *, *, #2108, .T. ) ;
#1017 = DIRECTION ( 'NONE',  ( 0.000000000000000000, 0.000000000000000000, -1.000000000000000000 ) ) ;
#1018 = ORIENTED_EDGE ( 'NONE', *, *, #2964, .T. ) ;
#1019 = EDGE_CURVE ( 'NONE', #7279, #2698, #8604, .T. ) ;
#1020 = PRODUCT_DEFINITION_CONTEXT ( 'detailed design', #8151, 'design' ) ;
#1021 = CARTESIAN_POINT ( 'NONE',  ( -16.29350689640810756, 140.5696653505793563, -10.98204862120179648 ) ) ;
#1022 = DIRECTION ( 'NONE',  ( -0.7071067811865431318, 8.659560562354989558E-17, -0.7071067811865520136 ) ) ;
#1023 = LINE ( 'NONE', #9891, #1119 ) ;
#1024 = DIRECTION ( 'NONE',  ( 0.000000000000000000, 1.000000000000000000, 0.000000000000000000 ) ) ;
#1025 = DIRECTION ( 'NONE',  ( -0.6691306063588565722, -0.7431448254773957984, 0.000000000000000000 ) ) ;
#1026 = EDGE_CURVE ( 'NONE', #8639, #6250, #10468, .T. ) ;
#1027 = DIRECTION ( 'NONE',  ( 0.000000000000000000, 0.000000000000000000, -1.000000000000000000 ) ) ;
#1028 = VERTEX_POINT ( 'NONE', #6354 ) ;
#1029 = FACE_OUTER_BOUND ( 'NONE', #6004, .T. ) ;
#1030 = EDGE_LOOP ( 'NONE', ( #7266, #4767, #8673, #8457 ) ) ;
#1031 = DIRECTION ( 'NONE',  ( 1.277197683604454965E-16, -1.000000000000000000, 0.000000000000000000 ) ) ;
#1032 = EDGE_LOOP ( 'NONE', ( #8944, #461, #7397, #6704 ) ) ;
#1033 = CARTESIAN_POINT ( 'NONE',  ( 97.72361618343356326, -145.1457019118818721, 30.00000000000000000 ) ) ;
#1034 = VECTOR ( 'NONE', #1710, 1000.000000000000000 ) ;
#1035 = CYLINDRICAL_SURFACE ( 'NONE', #1256, 4.000000000000000000 ) ;
#1036 = FACE_OUTER_BOUND ( 'NONE', #9629, .T. ) ;
#1037 = DIRECTION ( 'NONE',  ( -0.000000000000000000, 1.000000000000000000, -0.000000000000000000 ) ) ;
#1038 = CARTESIAN_POINT ( 'NONE',  ( -2.293506896408097795, 152.5696653505793279, -12.50000000000000000 ) ) ;
#1039 = DIRECTION ( 'NONE',  ( 0.000000000000000000, 0.000000000000000000, 1.000000000000000000 ) ) ;
#1040 = VERTEX_POINT ( 'NONE', #6300 ) ;
#1041 = VECTOR ( 'NONE', #1434, 1000.000000000000000 ) ;
#1042 = COLOUR_RGB ( '',0.7921568627450980005, 0.8196078431372548767, 0.9333333333333333481 ) ;
#1043 = VERTEX_POINT ( 'NONE', #1377 ) ;
#1044 = DIRECTION ( 'NONE',  ( 0.000000000000000000, -1.000000000000000000, 0.000000000000000000 ) ) ;
#1045 = CARTESIAN_POINT ( 'NONE',  ( -8.793506896408100459, 76.32362273389503571, 54.43095569077609497 ) ) ;
#1046 = CARTESIAN_POINT ( 'NONE',  ( -23.15769640663940976, -135.1457019118818721, 49.99999999999997868 ) ) ;
#1047 = LINE ( 'NONE', #4130, #10225 ) ;
#1048 = CYLINDRICAL_SURFACE ( 'NONE', #1606, 31.75575292317714471 ) ;
#1049 = VECTOR ( 'NONE', #861, 1000.000000000000000 ) ;
#1050 = CARTESIAN_POINT ( 'NONE',  ( 3.000000000000000000, -1.467624384280024730, 2.542000000000003368 ) ) ;
#1051 = VECTOR ( 'NONE', #4955, 1000.000000000000000 ) ;
#1052 = EDGE_CURVE ( 'NONE', #9925, #6648, #8435, .T. ) ;
#1053 = EDGE_CURVE ( 'NONE', #8741, #6235, #5555, .T. ) ;
#1054 = ORIENTED_EDGE ( 'NONE', *, *, #2979, .T. ) ;
#1055 = ORIENTED_EDGE ( 'NONE', *, *, #5527, .F. ) ;
#1056 = AXIS2_PLACEMENT_3D ( 'NONE', #10251, #6052, #6910 ) ;
#1057 = VERTEX_POINT ( 'NONE', #7843 ) ;
#1058 = AXIS2_PLACEMENT_3D ( 'NONE', #8553, #5110, #8811 ) ;
#1059 = CARTESIAN_POINT ( 'NONE',  ( -40.33539666817950575, 0.09126465619898900539, 4.000000000000000000 ) ) ;
#1060 = LINE ( 'NONE', #6623, #5109 ) ;
#1061 = FACE_OUTER_BOUND ( 'NONE', #2659, .T. ) ;
#1062 = CARTESIAN_POINT ( 'NONE',  ( -163.4029438717997209, 273.7745032373030085, 4.898587196589436495E-16 ) ) ;
#1063 = ORIENTED_EDGE ( 'NONE', *, *, #10418, .T. ) ;
#1064 = EDGE_CURVE ( 'NONE', #4776, #3587, #5889, .T. ) ;
#1065 = LINE ( 'NONE', #5988, #7731 ) ;
#1066 = EDGE_CURVE ( 'NONE', #9437, #7226, #4661, .T. ) ;
#1067 = CONICAL_SURFACE ( 'NONE', #8344, 4.999999999999993783, 1.029744258676652979 ) ;
#1068 = EDGE_CURVE ( 'NONE', #2989, #5742, #4960, .T. ) ;
#1069 = ORIENTED_EDGE ( 'NONE', *, *, #8198, .T. ) ;
#1070 = DIRECTION ( 'NONE',  ( 1.000000000000000000, 0.000000000000000000, 0.000000000000000000 ) ) ;
#1071 = ORIENTED_EDGE ( 'NONE', *, *, #664, .F. ) ;
#1072 = CARTESIAN_POINT ( 'NONE',  ( 3.000000000000000000, -1.467624384280024730, 2.542000000000003368 ) ) ;
#1073 = VECTOR ( 'NONE', #55, 1000.000000000000114 ) ;
#1074 = LINE ( 'NONE', #1819, #4670 ) ;
#1075 = PLANE ( 'NONE',  #7656 ) ;
#1076 = CARTESIAN_POINT ( 'NONE',  ( 3.000000000000000000, -1.467624384280024730, 2.542000000000003368 ) ) ;
#1077 = CYLINDRICAL_SURFACE ( 'NONE', #1290, 3.999999999999989786 ) ;
#1078 = EDGE_CURVE ( 'NONE', #9366, #5528, #100, .T. ) ;
#1079 = VERTEX_POINT ( 'NONE', #5656 ) ;
#1080 = LINE ( 'NONE', #1926, #7329 ) ;
#1081 = SHAPE_REPRESENTATION ( 'C-Frame Ductile Iron Housing', ( #4601 ), #9171 ) ;
#1082 = AXIS2_PLACEMENT_3D ( 'NONE', #1833, #6441, #9144 ) ;
#1083 = VERTEX_POINT ( 'NONE', #8893 ) ;
#1084 =( GEOMETRIC_REPRESENTATION_CONTEXT ( 3 ) GLOBAL_UNCERTAINTY_ASSIGNED_CONTEXT ( ( #4932 ) ) GLOBAL_UNIT_ASSIGNED_CONTEXT ( ( #1252, #7667, #5170 ) ) REPRESENTATION_CONTEXT ( 'NONE', 'WORKASPACE' ) );
#1085 = DIRECTION ( 'NONE',  ( 0.000000000000000000, 0.000000000000000000, 1.000000000000000000 ) ) ;
#1086 = ORIENTED_EDGE ( 'NONE', *, *, #8185, .T. ) ;
#1087 = AXIS2_PLACEMENT_3D ( 'NONE', #9894, #296, #2715 ) ;
#1088 = DIRECTION ( 'NONE',  ( 1.000000000000000000, -0.000000000000000000, -0.000000000000000000 ) ) ;
#1089 = DIRECTION ( 'NONE',  ( -0.7367503238654704578, -0.6761648913424330720, 0.000000000000000000 ) ) ;
#1090 = SPHERICAL_SURFACE ( 'NONE', #4333, 8.000000000000000000 ) ;
#1091 = CARTESIAN_POINT ( 'NONE',  ( -16.29350689640809691, -8.635287962196477096, 0.000000000000000000 ) ) ;
#1092 = ORIENTED_EDGE ( 'NONE', *, *, #2031, .F. ) ;
#1093 = AXIS2_PLACEMENT_3D ( 'NONE', #10384, #8834, #7151 ) ;
#1094 = LINE ( 'NONE', #313, #4102 ) ;
#1095 = ORIENTED_EDGE ( 'NONE', *, *, #6186, .T. ) ;
#1096 = AXIS2_PLACEMENT_3D ( 'NONE', #8801, #3977, #8692 ) ;
#1097 = CARTESIAN_POINT ( 'NONE',  ( -27.15769640663940976, -135.1457019118818721, 27.15769640663938489 ) ) ;
#1098 = EDGE_CURVE ( 'NONE', #7848, #8983, #5864, .T. ) ;
#1099 = CIRCLE ( 'NONE', #4798, 5.000000000000000000 ) ;
#1100 = ORIENTED_EDGE ( 'NONE', *, *, #4696, .T. ) ;
#1101 = CARTESIAN_POINT ( 'NONE',  ( -2.293506896408097795, 145.5696653505793563, -25.00000000000000711 ) ) ;
#1102 = DIRECTION ( 'NONE',  ( 1.000000000000000000, 0.000000000000000000, 0.000000000000000000 ) ) ;
#1103 = FILL_AREA_STYLE ('',( #2002 ) ) ;
#1104 = DIRECTION ( 'NONE',  ( 0.000000000000000000, 0.000000000000000000, -1.000000000000000000 ) ) ;
#1105 = CARTESIAN_POINT ( 'NONE',  ( -20.29350689640809691, 140.5696653505793563, 0.000000000000000000 ) ) ;
#1106 = CARTESIAN_POINT ( 'NONE',  ( 0.000000000000000000, -135.1457019118818721, -50.00000000000002132 ) ) ;
#1107 = TOROIDAL_SURFACE ( 'NONE', #8212, 4.000000000000000000, 2.000000000000000000 ) ;
#1108 = ORIENTED_EDGE ( 'NONE', *, *, #8919, .T. ) ;
#1109 = ORIENTED_EDGE ( 'NONE', *, *, #3823, .T. ) ;
#1110 = EDGE_CURVE ( 'NONE', #2425, #9911, #6741, .T. ) ;
#1111 = DIRECTION ( 'NONE',  ( -1.000000000000000000, 0.000000000000000000, 0.000000000000000000 ) ) ;
#1112 = CARTESIAN_POINT ( 'NONE',  ( -36.36957570605426326, 137.0132282531173473, 0.000000000000000000 ) ) ;
#1113 = CIRCLE ( 'NONE', #3829, 10.00000000000000178 ) ;
#1114 =( REPRESENTATION_RELATIONSHIP ('NONE','NONE', #9007, #9697 ) REPRESENTATION_RELATIONSHIP_WITH_TRANSFORMATION ( #9734 )SHAPE_REPRESENTATION_RELATIONSHIP( ) );
#1115 = CARTESIAN_POINT ( 'NONE',  ( -40.00000000000001421, -145.1457019118819005, -36.00000000000002842 ) ) ;
#1116 = LINE ( 'NONE', #7323, #6386 ) ;
#1117 = VERTEX_POINT ( 'NONE', #7257 ) ;
#1118 = DIRECTION ( 'NONE',  ( 0.000000000000000000, 0.000000000000000000, 1.000000000000000000 ) ) ;
#1119 = VECTOR ( 'NONE', #7385, 1000.000000000000000 ) ;
#1120 = ORIENTED_EDGE ( 'NONE', *, *, #5629, .T. ) ;
#1121 = VECTOR ( 'NONE', #863, 1000.000000000000000 ) ;
#1122 = ORIENTED_EDGE ( 'NONE', *, *, #7750, .F. ) ;
#1123 = ORIENTED_EDGE ( 'NONE', *, *, #8274, .F. ) ;
#1124 = EDGE_CURVE ( 'NONE', #4793, #490, #1337, .T. ) ;
#1125 = DIRECTION ( 'NONE',  ( 0.000000000000000000, 0.000000000000000000, -1.000000000000000000 ) ) ;
#1126 = DIRECTION ( 'NONE',  ( -1.000000000000000000, -0.000000000000000000, -0.000000000000000000 ) ) ;
#1127 = AXIS2_PLACEMENT_3D ( 'NONE', #6102, #496, #5361 ) ;
#1128 = EDGE_CURVE ( 'NONE', #5742, #6927, #4806, .T. ) ;
#1129 = LINE ( 'NONE', #1765, #4999 ) ;
#1130 = DIRECTION ( 'NONE',  ( -0.000000000000000000, 1.000000000000000000, -0.000000000000000000 ) ) ;
#1131 = CIRCLE ( 'NONE', #7064, 10.00000000000000888 ) ;
#1132 = DIRECTION ( 'NONE',  ( -1.000000000000000000, -0.000000000000000000, -0.000000000000000000 ) ) ;
#1133 = DIRECTION ( 'NONE',  ( 0.000000000000000000, 0.000000000000000000, 1.000000000000000000 ) ) ;
#1134 = ORIENTED_EDGE ( 'NONE', *, *, #9097, .T. ) ;
#1135 = DIRECTION ( 'NONE',  ( 0.000000000000000000, 0.000000000000000000, 1.000000000000000000 ) ) ;
#1136 = TOROIDAL_SURFACE ( 'NONE', #6889, 26.75575292317714471, 5.000000000000000000 ) ;
#1137 = EDGE_LOOP ( 'NONE', ( #3231, #9390, #5201, #9763 ) ) ;
#1138 = CARTESIAN_POINT ( 'NONE',  ( -155.4728935706336301, 261.2517229562222951, 0.000000000000000000 ) ) ;
#1139 = ORIENTED_EDGE ( 'NONE', *, *, #1019, .F. ) ;
#1140 = EDGE_CURVE ( 'NONE', #10264, #9816, #2426, .T. ) ;
#1141 = CIRCLE ( 'NONE', #800, 3.999999999999996447 ) ;
#1142 = CARTESIAN_POINT ( 'NONE',  ( -30.29350689640809335, 80.56966535057935630, 20.00000000000000711 ) ) ;
#1143 = CARTESIAN_POINT ( 'NONE',  ( 37.50928405972917545, -135.0885866703937097, 26.66685298234238033 ) ) ;
#1144 = CARTESIAN_POINT ( 'NONE',  ( 26.00000000000000355, 0.000000000000000000, 0.000000000000000000 ) ) ;
#1145 = DIRECTION ( 'NONE',  ( -1.000000000000000000, -0.000000000000000000, -0.000000000000000000 ) ) ;
#1146 = EDGE_LOOP ( 'NONE', ( #812, #8947 ) ) ;
#1147 = VECTOR ( 'NONE', #9282, 999.9999999999998863 ) ;
#1148 = CARTESIAN_POINT ( 'NONE',  ( -20.29350689640809691, 140.5696653505793563, 20.00000000000000355 ) ) ;
#1149 = VERTEX_POINT ( 'NONE', #4906 ) ;
#1150 = CARTESIAN_POINT ( 'NONE',  ( 0.000000000000000000, 0.000000000000000000, 0.000000000000000000 ) ) ;
#1151 = ORIENTED_EDGE ( 'NONE', *, *, #4635, .T. ) ;
#1152 = CIRCLE ( 'NONE', #3873, 4.000000000000000000 ) ;
#1153 = VECTOR ( 'NONE', #8174, 1000.000000000000000 ) ;
#1154 = DIRECTION ( 'NONE',  ( 0.000000000000000000, 1.000000000000000000, 0.000000000000000000 ) ) ;
#1155 = ORIENTED_EDGE ( 'NONE', *, *, #7944, .F. ) ;
#1156 = DIRECTION ( 'NONE',  ( -0.7431448254773957984, 0.6691306063588565722, -0.000000000000000000 ) ) ;
#1157 = CARTESIAN_POINT ( 'NONE',  ( -30.29350689640809335, 37.08684478514406635, 15.00000000000000355 ) ) ;
#1158 = PRESENTATION_STYLE_ASSIGNMENT (( #420 ) ) ;
#1159 = CARTESIAN_POINT ( 'NONE',  ( 23.15769640663939910, -117.1457019118819005, -48.00000000000002132 ) ) ;
#1160 = FACE_OUTER_BOUND ( 'NONE', #2223, .T. ) ;
#1161 = VECTOR ( 'NONE', #7788, 1000.000000000000000 ) ;
#1162 = DIRECTION ( 'NONE',  ( 0.000000000000000000, 0.000000000000000000, -1.000000000000000000 ) ) ;
#1163 = EDGE_CURVE ( 'NONE', #6235, #6817, #1738, .T. ) ;
#1164 = EDGE_LOOP ( 'NONE', ( #3662, #4158, #8425, #4498 ) ) ;
#1165 = CIRCLE ( 'NONE', #7936, 8.635821936424155965 ) ;
#1166 = VERTEX_POINT ( 'NONE', #785 ) ;
#1167 = ORIENTED_EDGE ( 'NONE', *, *, #8133, .T. ) ;
#1168 = CYLINDRICAL_SURFACE ( 'NONE', #6057, 2.000000000000001776 ) ;
#1169 = DIRECTION ( 'NONE',  ( 1.277197683604454965E-16, -1.000000000000000000, 0.000000000000000000 ) ) ;
#1170 = CONICAL_SURFACE ( 'NONE', #10140, 5.025000000000002132, 0.7853981633975176679 ) ;
#1171 = CARTESIAN_POINT ( 'NONE',  ( -50.00000000000001421, -135.1457019118818437, 26.27514435518735780 ) ) ;
#1172 = DIRECTION ( 'NONE',  ( 8.659560562356134638E-17, 0.7071067811864494290, -0.7071067811866454944 ) ) ;
#1173 = ORIENTED_EDGE ( 'NONE', *, *, #4710, .F. ) ;
#1174 = CYLINDRICAL_SURFACE ( 'NONE', #6372, 2.000000000000001776 ) ;
#1175 = EDGE_LOOP ( 'NONE', ( #6473, #7794, #10471, #9288 ) ) ;
#1176 = SURFACE_STYLE_FILL_AREA ( #5936 ) ;
#1177 = EDGE_CURVE ( 'NONE', #9448, #1323, #8204, .T. ) ;
#1178 = AXIS2_PLACEMENT_3D ( 'NONE', #4861, #5866, #5074 ) ;
#1179 = ORIENTED_EDGE ( 'NONE', *, *, #1098, .T. ) ;
#1180 = ORIENTED_EDGE ( 'NONE', *, *, #9874, .T. ) ;
#1181 = CARTESIAN_POINT ( 'NONE',  ( -2.293506896408101348, 37.08684478514406635, 25.00000000000000000 ) ) ;
#1182 = DIRECTION ( 'NONE',  ( 1.000000000000000000, 0.000000000000000000, -1.734723475976804383E-16 ) ) ;
#1183 = DIRECTION ( 'NONE',  ( -1.000000000000000000, 0.000000000000000000, 0.000000000000000000 ) ) ;
#1184 = DIRECTION ( 'NONE',  ( -0.6691306063588565722, -0.7431448254773956874, 0.000000000000000000 ) ) ;
#1185 = CARTESIAN_POINT ( 'NONE',  ( 14.70649310359190309, 80.56966535057935630, -20.00000000000000711 ) ) ;
#1186 = ORIENTED_EDGE ( 'NONE', *, *, #933, .F. ) ;
#1187 = CARTESIAN_POINT ( 'NONE',  ( -23.76520584195948516, -145.1457019118819005, -50.00000000000002132 ) ) ;
#1188 = EDGE_CURVE ( 'NONE', #2391, #1903, #4549, .T. ) ;
#1189 = ORIENTED_EDGE ( 'NONE', *, *, #3064, .F. ) ;
#1190 = DIRECTION ( 'NONE',  ( 0.000000000000000000, 0.000000000000000000, 1.000000000000000000 ) ) ;
#1191 = ORIENTED_EDGE ( 'NONE', *, *, #6603, .T. ) ;
#1192 = CYLINDRICAL_SURFACE ( 'NONE', #6034, 20.00000000000000000 ) ;
#1193 = FACE_OUTER_BOUND ( 'NONE', #1279, .T. ) ;
#1194 = CARTESIAN_POINT ( 'NONE',  ( -117.2684580747526581, 237.4318902223653254, 9.628383344360778382E-16 ) ) ;
#1195 = DIRECTION ( 'NONE',  ( 0.000000000000000000, -1.000000000000000000, 0.000000000000000000 ) ) ;
#1196 = ORIENTED_EDGE ( 'NONE', *, *, #1532, .F. ) ;
#1197 = DIRECTION ( 'NONE',  ( 0.000000000000000000, -0.000000000000000000, 1.000000000000000000 ) ) ;
#1198 = EDGE_CURVE ( 'NONE', #5466, #7089, #3190, .T. ) ;
#1199 = EDGE_CURVE ( 'NONE', #5863, #1913, #1792, .T. ) ;
#1200 = EDGE_CURVE ( 'NONE', #7910, #7087, #887, .T. ) ;
#1201 = ORIENTED_EDGE ( 'NONE', *, *, #1675, .T. ) ;
#1202 = ORIENTED_EDGE ( 'NONE', *, *, #8903, .F. ) ;
#1203 = CARTESIAN_POINT ( 'NONE',  ( 3.000000000000000000, 2.935248768560057897, -3.252606517456513302E-15 ) ) ;
#1204 = CIRCLE ( 'NONE', #8813, 2.000000000000001776 ) ;
#1205 = ORIENTED_EDGE ( 'NONE', *, *, #2933, .T. ) ;
#1206 = DIRECTION ( 'NONE',  ( 0.000000000000000000, -1.000000000000000000, -1.222897680782651224E-16 ) ) ;
#1207 = CARTESIAN_POINT ( 'NONE',  ( -16.29350689640809691, -8.660287962196477451, 0.000000000000000000 ) ) ;
#1208 = DIRECTION ( 'NONE',  ( 1.396588258780021135E-16, 0.000000000000000000, -1.000000000000000000 ) ) ;
#1209 = DIRECTION ( 'NONE',  ( 0.000000000000000000, 0.000000000000000000, -1.000000000000000000 ) ) ;
#1210 = CARTESIAN_POINT ( 'NONE',  ( -27.85255513972543895, 150.5696653505793563, 7.750000000000002665 ) ) ;
#1211 = LINE ( 'NONE', #1106, #9330 ) ;
#1212 = AXIS2_PLACEMENT_3D ( 'NONE', #9106, #4907, #8097 ) ;
#1213 = EDGE_CURVE ( 'NONE', #9582, #1239, #4026, .T. ) ;
#1214 = ORIENTED_EDGE ( 'NONE', *, *, #10303, .F. ) ;
#1215 = MECHANICAL_DESIGN_GEOMETRIC_PRESENTATION_REPRESENTATION (  '', ( #9163 ), #6451 ) ;
#1216 = ORIENTED_EDGE ( 'NONE', *, *, #225, .F. ) ;
#1217 = CARTESIAN_POINT ( 'NONE',  ( -23.15769640663937423, -133.1457019118818721, -50.00000000000002132 ) ) ;
#1218 = VERTEX_POINT ( 'NONE', #997 ) ;
#1219 = LINE ( 'NONE', #276, #5717 ) ;
#1220 = EDGE_CURVE ( 'NONE', #4525, #2500, #3708, .T. ) ;
#1221 = CYLINDRICAL_SURFACE ( 'NONE', #8153, 4.999999999999997335 ) ;
#1222 = VECTOR ( 'NONE', #6537, 1000.000000000000114 ) ;
#1223 = PRESENTATION_LAYER_ASSIGNMENT (  '', '', ( #3416 ) ) ;
#1224 = CARTESIAN_POINT ( 'NONE',  ( -16.29350689640809691, -186.9457019118818835, -27.01918567566963247 ) ) ;
#1225 = CARTESIAN_POINT ( 'NONE',  ( -2.293506896408097795, 150.5696653505793563, 20.00000000000000711 ) ) ;
#1226 = ORIENTED_EDGE ( 'NONE', *, *, #994, .F. ) ;
#1227 = ORIENTED_EDGE ( 'NONE', *, *, #7289, .T. ) ;
#1228 = AXIS2_PLACEMENT_3D ( 'NONE', #1345, #6962, #2821 ) ;
#1229 = AXIS2_PLACEMENT_3D ( 'NONE', #2526, #8196, #9147 ) ;
#1230 = EDGE_LOOP ( 'NONE', ( #6888, #8370, #3768, #8353 ) ) ;
#1231 = EDGE_LOOP ( 'NONE', ( #908, #3006, #6193, #9020 ) ) ;
#1232 = CARTESIAN_POINT ( 'NONE',  ( 17.97972049165455388, 37.08684478514406635, 30.00000000000000355 ) ) ;
#1233 = EDGE_CURVE ( 'NONE', #5528, #735, #9862, .T. ) ;
#1234 = DIRECTION ( 'NONE',  ( 0.000000000000000000, -1.431206729101514631E-16, 1.000000000000000000 ) ) ;
#1235 = CARTESIAN_POINT ( 'NONE',  ( -16.29350689640809691, -8.660287962196477451, 7.499999999999998224 ) ) ;
#1236 = CARTESIAN_POINT ( 'NONE',  ( -16.29350689640809691, 11.33971203780352255, 4.999999999999993783 ) ) ;
#1237 = AXIS2_PLACEMENT_3D ( 'NONE', #2653, #9877, #8163 ) ;
#1238 = CARTESIAN_POINT ( 'NONE',  ( 6.250000000000005329, 3.673940397442060361E-16, -3.000000000000000444 ) ) ;
#1239 = VERTEX_POINT ( 'NONE', #160 ) ;
#1240 = VECTOR ( 'NONE', #5404, 1000.000000000000000 ) ;
#1241 = DIRECTION ( 'NONE',  ( -8.194486552889013533E-17, -9.100899318238110877E-17, 1.000000000000000000 ) ) ;
#1242 = CARTESIAN_POINT ( 'NONE',  ( -40.00000000000001421, -135.1707019118818778, -40.00000000000002132 ) ) ;
#1243 = EDGE_CURVE ( 'NONE', #1644, #2082, #5896, .T. ) ;
#1244 = DIRECTION ( 'NONE',  ( -1.000000000000000000, 0.000000000000000000, 0.000000000000000000 ) ) ;
#1245 = DIRECTION ( 'NONE',  ( -1.000000000000000000, 0.000000000000000000, 0.000000000000000000 ) ) ;
#1246 = DIRECTION ( 'NONE',  ( -0.6691306063588565722, -0.7431448254773957984, 0.000000000000000000 ) ) ;
#1247 = VECTOR ( 'NONE', #1264, 1000.000000000000000 ) ;
#1248 = DIRECTION ( 'NONE',  ( 0.000000000000000000, 0.000000000000000000, 1.000000000000000000 ) ) ;
#1249 = ORIENTED_EDGE ( 'NONE', *, *, #7540, .T. ) ;
#1250 = CARTESIAN_POINT ( 'NONE',  ( -40.00000000000001421, -115.1457019118818863, -40.00000000000002132 ) ) ;
#1251 = ORIENTED_EDGE ( 'NONE', *, *, #4194, .T. ) ;
#1252 =( LENGTH_UNIT ( ) NAMED_UNIT ( * ) SI_UNIT ( .MILLI., .METRE. ) );
#1253 = VERTEX_POINT ( 'NONE', #6505 ) ;
#1254 = DIRECTION ( 'NONE',  ( 0.000000000000000000, -0.000000000000000000, 1.000000000000000000 ) ) ;
#1255 = ORIENTED_EDGE ( 'NONE', *, *, #475, .T. ) ;
#1256 = AXIS2_PLACEMENT_3D ( 'NONE', #4271, #9252, #4325 ) ;
#1257 = ORIENTED_EDGE ( 'NONE', *, *, #4817, .F. ) ;
#1258 = LINE ( 'NONE', #2847, #104 ) ;
#1259 = ADVANCED_FACE ( 'NONE', ( #9754 ), #6405, .T. ) ;
#1260 = DIRECTION ( 'NONE',  ( 1.000000000000000000, 0.000000000000000000, -0.000000000000000000 ) ) ;
#1261 = ADVANCED_FACE ( 'NONE', ( #3434 ), #6878, .T. ) ;
#1262 = EDGE_CURVE ( 'NONE', #4871, #8587, #6077, .T. ) ;
#1263 = DIRECTION ( 'NONE',  ( -1.000000000000000000, -0.000000000000000000, -0.000000000000000000 ) ) ;
#1264 = DIRECTION ( 'NONE',  ( 1.000000000000000000, -0.000000000000000000, -0.000000000000000000 ) ) ;
#1265 = PLANE ( 'NONE',  #6164 ) ;
#1266 = CARTESIAN_POINT ( 'NONE',  ( -16.29350689640809691, 105.5289575273812233, -7.750000000000000000 ) ) ;
#1267 = AXIS2_PLACEMENT_3D ( 'NONE', #9632, #508, #5320 ) ;
#1268 = EDGE_LOOP ( 'NONE', ( #3343, #2802, #567, #512, #4602, #10138, #10269 ) ) ;
#1269 = ORIENTED_EDGE ( 'NONE', *, *, #5144, .T. ) ;
#1270 = DIRECTION ( 'NONE',  ( 0.000000000000000000, 0.4226182617406934461, 0.9063077870366527122 ) ) ;
#1271 = AXIS2_PLACEMENT_3D ( 'NONE', #6457, #8000, #8045 ) ;
#1272 = ORIENTED_EDGE ( 'NONE', *, *, #10189, .T. ) ;
#1273 = DIRECTION ( 'NONE',  ( 0.000000000000000000, 0.7071067811864494290, 0.7071067811866454944 ) ) ;
#1274 = CARTESIAN_POINT ( 'NONE',  ( 42.22511195853866894, 17.84145331825995484, -25.00000000000000355 ) ) ;
#1275 = EDGE_CURVE ( 'NONE', #6869, #10235, #6919, .T. ) ;
#1276 = DIRECTION ( 'NONE',  ( 1.000000000000000000, -0.000000000000000000, -0.000000000000000000 ) ) ;
#1277 = DIRECTION ( 'NONE',  ( 0.000000000000000000, 0.000000000000000000, -1.000000000000000000 ) ) ;
#1278 = AXIS2_PLACEMENT_3D ( 'NONE', #5647, #4167, #987 ) ;
#1279 = EDGE_LOOP ( 'NONE', ( #3702, #9720, #2445, #3175 ) ) ;
#1280 = ORIENTED_EDGE ( 'NONE', *, *, #4742, .F. ) ;
#1281 = AXIS2_PLACEMENT_3D ( 'NONE', #3694, #405, #1246 ) ;
#1282 = VERTEX_POINT ( 'NONE', #9970 ) ;
#1283 = ORIENTED_EDGE ( 'NONE', *, *, #6820, .F. ) ;
#1284 = FACE_OUTER_BOUND ( 'NONE', #3777, .T. ) ;
#1285 = DIRECTION ( 'NONE',  ( 0.000000000000000000, -0.000000000000000000, -1.000000000000000000 ) ) ;
#1286 = CARTESIAN_POINT ( 'NONE',  ( 59.99999999999997868, -145.1457019118819005, 30.00000000000000355 ) ) ;
#1287 = DIRECTION ( 'NONE',  ( 1.000000000000000000, 0.000000000000000000, -0.000000000000000000 ) ) ;
#1288 = AXIS2_PLACEMENT_3D ( 'NONE', #6719, #5175, #10061 ) ;
#1289 = LINE ( 'NONE', #10253, #8564 ) ;
#1290 = AXIS2_PLACEMENT_3D ( 'NONE', #2028, #2769, #4415 ) ;
#1291 = EDGE_LOOP ( 'NONE', ( #7966, #7553 ) ) ;
#1292 = CARTESIAN_POINT ( 'NONE',  ( -40.99999999999999289, 3.464101615137777923, -1.999999999999970468 ) ) ;
#1293 = EDGE_CURVE ( 'NONE', #1886, #7279, #2790, .T. ) ;
#1294 = CARTESIAN_POINT ( 'NONE',  ( -18.34874108452141783, -140.1746510883711778, -97.78965767959371647 ) ) ;
#1295 = ORIENTED_EDGE ( 'NONE', *, *, #7737, .F. ) ;
#1296 = TOROIDAL_SURFACE ( 'NONE', #961, 12.02085523418795177, 4.295524112943378547 ) ;
#1297 = CARTESIAN_POINT ( 'NONE',  ( -50.00000000000002842, -135.1457019118818721, 39.99999999999997868 ) ) ;
#1298 = CARTESIAN_POINT ( 'NONE',  ( 24.41868145091757825, -134.3099331815685105, -50.00000000000001421 ) ) ;
#1299 = DIRECTION ( 'NONE',  ( 9.776117811460147207E-16, 0.000000000000000000, -1.000000000000000000 ) ) ;
#1300 = VECTOR ( 'NONE', #2207, 1000.000000000000114 ) ;
#1301 = ORIENTED_EDGE ( 'NONE', *, *, #3401, .T. ) ;
#1302 = DIRECTION ( 'NONE',  ( 1.000000000000000000, -0.000000000000000000, -0.000000000000000000 ) ) ;
#1303 = CIRCLE ( 'NONE', #9779, 2.000000000000001776 ) ;
#1304 = VERTEX_POINT ( 'NONE', #2691 ) ;
#1305 = APPLICATION_PROTOCOL_DEFINITION ( 'draft international standard', 'automotive_design', 1998, #4085 ) ;
#1306 = EDGE_CURVE ( 'NONE', #7774, #6869, #7551, .T. ) ;
#1307 = ORIENTED_EDGE ( 'NONE', *, *, #1584, .F. ) ;
#1308 = LINE ( 'NONE', #6177, #5194 ) ;
#1309 = ORIENTED_EDGE ( 'NONE', *, *, #6248, .F. ) ;
#1310 = CIRCLE ( 'NONE', #9272, 2.000000000000001776 ) ;
#1311 = ORIENTED_EDGE ( 'NONE', *, *, #2487, .F. ) ;
#1312 = LINE ( 'NONE', #7938, #10266 ) ;
#1313 = CARTESIAN_POINT ( 'NONE',  ( 0.000000000000000000, 1.467624384280025174, -2.542000000000001592 ) ) ;
#1314 = VERTEX_POINT ( 'NONE', #7515 ) ;
#1315 = CARTESIAN_POINT ( 'NONE',  ( -30.29350689640809335, 120.5696653505793705, -20.00000000000000711 ) ) ;
#1316 = VECTOR ( 'NONE', #1172, 1000.000000000000000 ) ;
#1317 = DIRECTION ( 'NONE',  ( -1.000000000000000000, -0.000000000000000000, -0.000000000000000000 ) ) ;
#1318 = FACE_OUTER_BOUND ( 'NONE', #283, .T. ) ;
#1319 = DIRECTION ( 'NONE',  ( 1.000000000000000000, 0.000000000000000000, -0.000000000000000000 ) ) ;
#1320 = VECTOR ( 'NONE', #1750, 1000.000000000000000 ) ;
#1321 =( REPRESENTATION_RELATIONSHIP ('NONE','NONE', #9007, #286 ) REPRESENTATION_RELATIONSHIP_WITH_TRANSFORMATION ( #4997 )SHAPE_REPRESENTATION_RELATIONSHIP( ) );
#1322 = EDGE_CURVE ( 'NONE', #10164, #4525, #1258, .T. ) ;
#1323 = VERTEX_POINT ( 'NONE', #9105 ) ;
#1324 = EDGE_CURVE ( 'NONE', #2102, #8741, #3648, .T. ) ;
#1325 = LINE ( 'NONE', #9490, #4345 ) ;
#1326 = ORIENTED_EDGE ( 'NONE', *, *, #5527, .T. ) ;
#1327 = LINE ( 'NONE', #9223, #1666 ) ;
#1328 = VECTOR ( 'NONE', #3333, 1000.000000000000000 ) ;
#1329 = ORIENTED_EDGE ( 'NONE', *, *, #3402, .T. ) ;
#1330 = CARTESIAN_POINT ( 'NONE',  ( 37.59878849545336266, 37.08684478514405214, -12.50000000000000000 ) ) ;
#1331 = DIRECTION ( 'NONE',  ( 0.000000000000000000, 0.000000000000000000, 1.000000000000000000 ) ) ;
#1332 = LINE ( 'NONE', #9995, #7522 ) ;
#1333 = ORIENTED_EDGE ( 'NONE', *, *, #9472, .T. ) ;
#1334 = ORIENTED_EDGE ( 'NONE', *, *, #1987, .T. ) ;
#1335 = ADVANCED_FACE ( 'NONE', ( #9320 ), #1892, .T. ) ;
#1336 = EDGE_CURVE ( 'NONE', #8252, #7910, #7889, .T. ) ;
#1337 = CIRCLE ( 'NONE', #2348, 8.855570079111213744 ) ;
#1338 = ADVANCED_FACE ( 'NONE', ( #265 ), #10168, .F. ) ;
#1339 = ORIENTED_EDGE ( 'NONE', *, *, #1006, .F. ) ;
#1340 = VECTOR ( 'NONE', #10000, 1000.000000000000000 ) ;
#1341 = ORIENTED_EDGE ( 'NONE', *, *, #6759, .T. ) ;
#1342 = DIRECTION ( 'NONE',  ( -1.000000000000000000, 0.000000000000000000, -0.000000000000000000 ) ) ;
#1343 = FACE_OUTER_BOUND ( 'NONE', #311, .T. ) ;
#1344 = CYLINDRICAL_SURFACE ( 'NONE', #2810, 3.999999999999989786 ) ;
#1345 = CARTESIAN_POINT ( 'NONE',  ( 27.15769640663936713, -117.1457019118819005, 23.15769640663938134 ) ) ;
#1346 = CARTESIAN_POINT ( 'NONE',  ( 0.000000000000000000, -135.1457019118818721, 0.000000000000000000 ) ) ;
#1347 = ORIENTED_EDGE ( 'NONE', *, *, #1675, .F. ) ;
#1348 = VECTOR ( 'NONE', #6045, 1000.000000000000000 ) ;
#1349 = CARTESIAN_POINT ( 'NONE',  ( 17.97972049165455388, 17.84145331825995484, 30.00000000000000355 ) ) ;
#1350 = ADVANCED_FACE ( 'NONE', ( #2740 ), #3703, .T. ) ;
#1351 = LINE ( 'NONE', #3687, #3374 ) ;
#1352 = VERTEX_POINT ( 'NONE', #8306 ) ;
#1353 = EDGE_CURVE ( 'NONE', #9176, #941, #4338, .T. ) ;
#1354 = CARTESIAN_POINT ( 'NONE',  ( -7.293506896408097795, 126.8146633489777599, 25.00000000000000355 ) ) ;
#1355 = DIRECTION ( 'NONE',  ( -0.000000000000000000, -0.000000000000000000, -1.000000000000000000 ) ) ;
#1356 = FACE_OUTER_BOUND ( 'NONE', #10389, .T. ) ;
#1357 = ORIENTED_EDGE ( 'NONE', *, *, #2172, .F. ) ;
#1358 = DIRECTION ( 'NONE',  ( -0.000000000000000000, 1.000000000000000000, -0.000000000000000000 ) ) ;
#1359 = VERTEX_POINT ( 'NONE', #1101 ) ;
#1360 = DIRECTION ( 'NONE',  ( 1.000000000000000000, -2.775557561562891351E-17, 1.110223024625156787E-16 ) ) ;
#1361 = ORIENTED_EDGE ( 'NONE', *, *, #5317, .F. ) ;
#1362 = DIRECTION ( 'NONE',  ( 0.000000000000000000, 1.000000000000000000, 0.000000000000000000 ) ) ;
#1363 = EDGE_LOOP ( 'NONE', ( #3684, #2571, #10349, #9047 ) ) ;
#1364 = EDGE_LOOP ( 'NONE', ( #8851, #10286, #468 ) ) ;
#1365 = FACE_OUTER_BOUND ( 'NONE', #3229, .T. ) ;
#1366 = SPHERICAL_SURFACE ( 'NONE', #6302, 2.000000000000000000 ) ;
#1367 = EDGE_LOOP ( 'NONE', ( #7375, #167, #6674, #5877 ) ) ;
#1368 = FILL_AREA_STYLE ('',( #8625 ) ) ;
#1369 = DIRECTION ( 'NONE',  ( 1.000000000000000000, 0.000000000000000000, 0.000000000000000000 ) ) ;
#1370 = CARTESIAN_POINT ( 'NONE',  ( -16.26850689640809478, 140.5696653505793563, 20.00000000000002132 ) ) ;
#1371 = CARTESIAN_POINT ( 'NONE',  ( -16.29350689640809691, 81.26698356513965393, 0.000000000000000000 ) ) ;
#1372 = CARTESIAN_POINT ( 'NONE',  ( -33.96613322994402751, 137.0132282531173473, 0.000000000000000000 ) ) ;
#1373 = EDGE_LOOP ( 'NONE', ( #7670, #9589 ) ) ;
#1374 = DIRECTION ( 'NONE',  ( 0.000000000000000000, -1.000000000000000000, 0.000000000000000000 ) ) ;
#1375 = AXIS2_PLACEMENT_3D ( 'NONE', #1266, #7628, #6776 ) ;
#1376 = ORIENTED_EDGE ( 'NONE', *, *, #3788, .T. ) ;
#1377 = CARTESIAN_POINT ( 'NONE',  ( -16.29350689640809691, 55.56966535057936341, -7.500000000000000000 ) ) ;
#1378 =( NAMED_UNIT ( * ) SI_UNIT ( $, .STERADIAN. ) SOLID_ANGLE_UNIT ( ) );
#1379 = DIRECTION ( 'NONE',  ( -0.000000000000000000, 1.000000000000000000, 0.000000000000000000 ) ) ;
#1380 = EDGE_CURVE ( 'NONE', #8244, #9480, #7671, .T. ) ;
#1381 = DIRECTION ( 'NONE',  ( 0.000000000000000000, 0.000000000000000000, 1.000000000000000000 ) ) ;
#1382 = CIRCLE ( 'NONE', #2725, 2.000000000000001776 ) ;
#1383 = CARTESIAN_POINT ( 'NONE',  ( -117.0000000000000000, 0.000000000000000000, 0.000000000000000000 ) ) ;
#1384 = VECTOR ( 'NONE', #4482, 1000.000000000000227 ) ;
#1385 = ORIENTED_EDGE ( 'NONE', *, *, #287, .F. ) ;
#1386 = VERTEX_POINT ( 'NONE', #3486 ) ;
#1387 = AXIS2_PLACEMENT_3D ( 'NONE', #1488, #7206, #7899 ) ;
#1388 = ORIENTED_EDGE ( 'NONE', *, *, #5728, .T. ) ;
#1389 = AXIS2_PLACEMENT_3D ( 'NONE', #3350, #4083, #9715 ) ;
#1390 = ORIENTED_EDGE ( 'NONE', *, *, #7674, .F. ) ;
#1391 = CARTESIAN_POINT ( 'NONE',  ( -56.36957570605427037, 137.0132282531173473, 0.000000000000000000 ) ) ;
#1392 = DIRECTION ( 'NONE',  ( -0.000000000000000000, 1.000000000000000000, -0.000000000000000000 ) ) ;
#1393 = LINE ( 'NONE', #3729, #6363 ) ;
#1394 = CARTESIAN_POINT ( 'NONE',  ( 32.59878849545336976, 32.08684478514406635, 12.50000000000000355 ) ) ;
#1395 = EDGE_CURVE ( 'NONE', #9655, #10447, #7716, .T. ) ;
#1396 = ADVANCED_FACE ( 'NONE', ( #3593 ), #9212, .F. ) ;
#1397 = ADVANCED_FACE ( 'NONE', ( #10012 ), #3914, .T. ) ;
#1398 = CARTESIAN_POINT ( 'NONE',  ( 14.70649310359190309, 80.56966535057935630, 16.00000000000000711 ) ) ;
#1399 = CONICAL_SURFACE ( 'NONE', #5616, 6.499999999999964473, 0.7853981633974560506 ) ;
#1400 = ORIENTED_EDGE ( 'NONE', *, *, #2979, .F. ) ;
#1401 = TOROIDAL_SURFACE ( 'NONE', #8656, 4.000000000000000000, 2.000000000000000000 ) ;
#1402 = DIRECTION ( 'NONE',  ( -0.6691306063588565722, -0.7431448254773956874, 0.000000000000000000 ) ) ;
#1403 = VERTEX_POINT ( 'NONE', #3862 ) ;
#1404 = LINE ( 'NONE', #8769, #9445 ) ;
#1405 = CIRCLE ( 'NONE', #52, 5.000000000000000888 ) ;
#1406 = VECTOR ( 'NONE', #3370, 1000.000000000000000 ) ;
#1407 = ADVANCED_FACE ( 'NONE', ( #3750 ), #2157, .T. ) ;
#1408 = DIRECTION ( 'NONE',  ( -0.7525569905852198538, -0.6585271261848804070, 0.000000000000000000 ) ) ;
#1409 = DIRECTION ( 'NONE',  ( 0.000000000000000000, 0.000000000000000000, 1.000000000000000000 ) ) ;
#1410 = CARTESIAN_POINT ( 'NONE',  ( 85.07264007511442117, 55.10093597859600578, 30.00000000000000355 ) ) ;
#1411 = ORIENTED_EDGE ( 'NONE', *, *, #6341, .T. ) ;
#1412 = CARTESIAN_POINT ( 'NONE',  ( 37.22511195853868315, -117.1457019118819005, 23.15769640663938134 ) ) ;
#1413 = VECTOR ( 'NONE', #6522, 1000.000000000000000 ) ;
#1414 = DIRECTION ( 'NONE',  ( 1.000000000000000000, 7.285838599102589797E-17, -5.551115123125782702E-17 ) ) ;
#1415 = ORIENTED_EDGE ( 'NONE', *, *, #7981, .F. ) ;
#1416 = CARTESIAN_POINT ( 'NONE',  ( -16.29350689640809691, -140.1746510883711778, 27.01918567566963247 ) ) ;
#1417 = ORIENTED_EDGE ( 'NONE', *, *, #8566, .F. ) ;
#1418 = ORIENTED_EDGE ( 'NONE', *, *, #9964, .T. ) ;
#1419 = DIRECTION ( 'NONE',  ( 1.000000000000000000, 0.000000000000000000, 0.000000000000000000 ) ) ;
#1420 = CARTESIAN_POINT ( 'NONE',  ( 10.51964330236497602, 150.0000000000000000, 12.50000000000000355 ) ) ;
#1421 = AXIS2_PLACEMENT_3D ( 'NONE', #9108, #7361, #5075 ) ;
#1422 = DIRECTION ( 'NONE',  ( 1.000000000000000000, 0.000000000000000000, -0.000000000000000000 ) ) ;
#1423 = DIRECTION ( 'NONE',  ( 0.000000000000000000, 0.000000000000000000, 1.000000000000000000 ) ) ;
#1424 = DIRECTION ( 'NONE',  ( -0.7431448254773957984, 0.6691306063588565722, -0.000000000000000000 ) ) ;
#1425 = DIRECTION ( 'NONE',  ( 0.000000000000000000, 1.000000000000000000, 0.000000000000000000 ) ) ;
#1426 = CARTESIAN_POINT ( 'NONE',  ( -16.29350689640809691, 11.33971203780352255, -4.999999999999993783 ) ) ;
#1427 = EDGE_CURVE ( 'NONE', #5184, #10246, #5343, .T. ) ;
#1428 = ORIENTED_EDGE ( 'NONE', *, *, #6311, .F. ) ;
#1429 = VECTOR ( 'NONE', #8033, 1000.000000000000000 ) ;
#1430 = DIRECTION ( 'NONE',  ( 0.000000000000000000, 1.000000000000000000, -1.329743448921560837E-15 ) ) ;
#1431 = PRODUCT_DEFINITION_FORMATION_WITH_SPECIFIED_SOURCE ( 'ANY', '', #2472, .NOT_KNOWN. ) ;
#1432 = ORIENTED_EDGE ( 'NONE', *, *, #5788, .T. ) ;
#1433 = DIRECTION ( 'NONE',  ( 0.000000000000000000, 0.000000000000000000, 1.000000000000000000 ) ) ;
#1434 = DIRECTION ( 'NONE',  ( -0.000000000000000000, -0.000000000000000000, 1.000000000000000000 ) ) ;
#1435 = DIRECTION ( 'NONE',  ( -3.081165567444019513E-16, 1.000000000000000000, 0.000000000000000000 ) ) ;
#1436 = DIRECTION ( 'NONE',  ( -0.000000000000000000, -0.000000000000000000, 1.000000000000000000 ) ) ;
#1437 = CARTESIAN_POINT ( 'NONE',  ( 23.15769640663940265, -117.1457019118819005, -48.00000000000002132 ) ) ;
#1438 = ORIENTED_EDGE ( 'NONE', *, *, #7942, .T. ) ;
#1439 = VERTEX_POINT ( 'NONE', #8785 ) ;
#1440 = EDGE_CURVE ( 'NONE', #9059, #10117, #7146, .T. ) ;
#1441 = CIRCLE ( 'NONE', #6166, 7.794205612481196255 ) ;
#1442 = ORIENTED_EDGE ( 'NONE', *, *, #5543, .T. ) ;
#1443 = VERTEX_POINT ( 'NONE', #6181 ) ;
#1444 = CYLINDRICAL_SURFACE ( 'NONE', #9626, 3.999999999999989786 ) ;
#1445 = DIRECTION ( 'NONE',  ( -0.000000000000000000, 1.000000000000000000, -0.000000000000000000 ) ) ;
#1446 = VECTOR ( 'NONE', #164, 1000.000000000000000 ) ;
#1447 = CARTESIAN_POINT ( 'NONE',  ( -20.14472382240651172, -141.8229441850657793, -28.16739522765907111 ) ) ;
#1448 = DIRECTION ( 'NONE',  ( -0.7431448254773957984, 0.6691306063588565722, -0.000000000000000000 ) ) ;
#1449 = DIRECTION ( 'NONE',  ( -1.000000000000000000, -0.000000000000000000, -0.000000000000000000 ) ) ;
#1450 = ORIENTED_EDGE ( 'NONE', *, *, #6573, .T. ) ;
#1451 = DIRECTION ( 'NONE',  ( 0.000000000000000000, 0.000000000000000000, 1.000000000000000000 ) ) ;
#1452 = AXIS2_PLACEMENT_3D ( 'NONE', #8678, #4652, #9540 ) ;
#1453 = EDGE_CURVE ( 'NONE', #10419, #9834, #8224, .T. ) ;
#1454 = EDGE_CURVE ( 'NONE', #5461, #6490, #1312, .T. ) ;
#1455 = VERTEX_POINT ( 'NONE', #8622 ) ;
#1456 = EDGE_CURVE ( 'NONE', #9556, #5912, #2801, .T. ) ;
#1457 = DIRECTION ( 'NONE',  ( 1.137729606058012035E-16, 0.000000000000000000, 1.000000000000000000 ) ) ;
#1458 = AXIS2_PLACEMENT_3D ( 'NONE', #9422, #3108, #10330 ) ;
#1459 = PRODUCT_DEFINITION_SHAPE ( 'NONE', 'NONE',  #10479 ) ;
#1460 = AXIS2_PLACEMENT_3D ( 'NONE', #7974, #8818, #5585 ) ;
#1461 = DIRECTION ( 'NONE',  ( -0.9805806756909200006, -0.1698415551216896080, -0.09805806756909324351 ) ) ;
#1462 = CARTESIAN_POINT ( 'NONE',  ( -8.793506896408096907, 120.5289575273812233, -7.750000000000000000 ) ) ;
#1463 = CARTESIAN_POINT ( 'NONE',  ( -40.00000000000001421, -135.1457019118818721, -44.00000000000001421 ) ) ;
#1464 = ORIENTED_EDGE ( 'NONE', *, *, #8642, .T. ) ;
#1465 = DIRECTION ( 'NONE',  ( 0.000000000000000000, 0.000000000000000000, 1.000000000000000000 ) ) ;
#1466 = VECTOR ( 'NONE', #6032, 1000.000000000000000 ) ;
#1468 = ADVANCED_FACE ( 'NONE', ( #1526 ), #3056, .T. ) ;
#1467 = EDGE_LOOP ( 'NONE', ( #2773, #217, #5935, #2397 ) ) ;
#1469 = VECTOR ( 'NONE', #602, 1000.000000000000000 ) ;
#1470 = ADVANCED_FACE ( 'NONE', ( #1365 ), #4593, .T. ) ;
#1471 = DIRECTION ( 'NONE',  ( -1.000000000000000000, 0.000000000000000000, 0.000000000000000000 ) ) ;
#1472 = ORIENTED_EDGE ( 'NONE', *, *, #9893, .F. ) ;
#1473 = ORIENTED_EDGE ( 'NONE', *, *, #4035, .F. ) ;
#1474 = DIRECTION ( 'NONE',  ( 0.000000000000000000, 0.000000000000000000, 1.000000000000000000 ) ) ;
#1475 = CONICAL_SURFACE ( 'NONE', #10448, 4.025000000000000355, 0.7853981633975870569 ) ;
#1476 = CYLINDRICAL_SURFACE ( 'NONE', #305, 2.000000000000001776 ) ;
#1477 = DIRECTION ( 'NONE',  ( -0.000000000000000000, -0.000000000000000000, 1.000000000000000000 ) ) ;
#1478 = DIRECTION ( 'NONE',  ( 1.000000000000000000, 0.000000000000000000, 8.379529552680125332E-16 ) ) ;
#1479 = VECTOR ( 'NONE', #6419, 1000.000000000000000 ) ;
#1480 = VECTOR ( 'NONE', #8113, 1000.000000000000000 ) ;
#1481 = DIRECTION ( 'NONE',  ( -0.000000000000000000, 1.222897680782651471E-16, -1.000000000000000000 ) ) ;
#1482 = ORIENTED_EDGE ( 'NONE', *, *, #10425, .F. ) ;
#1483 = AXIS2_PLACEMENT_3D ( 'NONE', #3362, #5892, #1867 ) ;
#1484 = PLANE ( 'NONE',  #7384 ) ;
#1485 = VECTOR ( 'NONE', #3097, 1000.000000000000000 ) ;
#1486 = ORIENTED_EDGE ( 'NONE', *, *, #3167, .T. ) ;
#1487 = DIRECTION ( 'NONE',  ( 0.000000000000000000, 1.000000000000000000, 0.000000000000000000 ) ) ;
#1488 = CARTESIAN_POINT ( 'NONE',  ( 17.97972049165455388, 17.84145331825995484, 25.00000000000000000 ) ) ;
#1489 = CARTESIAN_POINT ( 'NONE',  ( -1.071796769724492338, 0.000000000000000000, 0.000000000000000000 ) ) ;
#1490 = EDGE_CURVE ( 'NONE', #490, #4793, #9756, .T. ) ;
#1491 = EDGE_CURVE ( 'NONE', #5933, #4432, #4268, .T. ) ;
#1492 = DIRECTION ( 'NONE',  ( 0.000000000000000000, -0.7071067811864985009, -0.7071067811865965336 ) ) ;
#1493 = AXIS2_PLACEMENT_3D ( 'NONE', #9562, #3939, #4675 ) ;
#1494 = DIRECTION ( 'NONE',  ( 0.1124875939035006184, 0.07750954751060692982, -0.9906254646749710346 ) ) ;
#1495 = EDGE_LOOP ( 'NONE', ( #1173, #10130, #3801, #3859 ) ) ;
#1496 = ORIENTED_EDGE ( 'NONE', *, *, #7467, .T. ) ;
#1497 = AXIS2_PLACEMENT_3D ( 'NONE', #4715, #3173, #2224 ) ;
#1498 = EDGE_LOOP ( 'NONE', ( #3886, #8646, #4986, #9342 ) ) ;
#1499 = CARTESIAN_POINT ( 'NONE',  ( -50.00000000000002132, -134.6884840344297913, -24.98777100551304997 ) ) ;
#1500 = DIRECTION ( 'NONE',  ( 0.000000000000000000, -1.000000000000000000, 0.000000000000000000 ) ) ;
#1501 = AXIS2_PLACEMENT_3D ( 'NONE', #5590, #8724, #1471 ) ;
#1502 = CARTESIAN_POINT ( 'NONE',  ( 80.08610854271792334, 54.73418909528891874, -30.00000000000000355 ) ) ;
#1503 = FACE_OUTER_BOUND ( 'NONE', #5938, .T. ) ;
#1504 = ORIENTED_EDGE ( 'NONE', *, *, #3206, .T. ) ;
#1505 = CYLINDRICAL_SURFACE ( 'NONE', #3325, 10.00000000000000178 ) ;
#1506 = AXIS2_PLACEMENT_3D ( 'NONE', #8795, #1487, #7898 ) ;
#1507 = ORIENTED_EDGE ( 'NONE', *, *, #3207, .T. ) ;
#1508 = CARTESIAN_POINT ( 'NONE',  ( -16.29350689640809691, 105.5289575273812233, -25.04213562373096380 ) ) ;
#1509=STYLED_ITEM('',(#10518),#2958);
#1510 = ORIENTED_EDGE ( 'NONE', *, *, #3911, .F. ) ;
#1511 = PLANE ( 'NONE',  #6559 ) ;
#1512 = UNCERTAINTY_MEASURE_WITH_UNIT (LENGTH_MEASURE( 1.000000000000000082E-05 ), #2813, 'distance_accuracy_value', 'NONE');
#1513 = CARTESIAN_POINT ( 'NONE',  ( -16.29350689640809691, 81.26698356513965393, 0.000000000000000000 ) ) ;
#1514 = AXIS2_PLACEMENT_3D ( 'NONE', #2760, #5991, #9233 ) ;
#1515 = CARTESIAN_POINT ( 'NONE',  ( 24.98777100551300023, -134.6884840344297913, -50.00000000000002132 ) ) ;
#1516 = EDGE_CURVE ( 'NONE', #2007, #1282, #9590, .T. ) ;
#1517 = CARTESIAN_POINT ( 'NONE',  ( -31.74999999999995737, 0.000000000000000000, 0.000000000000000000 ) ) ;
#1518 = VERTEX_POINT ( 'NONE', #9535 ) ;
#1519 = CARTESIAN_POINT ( 'NONE',  ( -16.26850689640809833, 140.5696653505793563, -7.749999999999996447 ) ) ;
#1520 = PRODUCT_CONTEXT ( 'NONE', #1525, 'mechanical' ) ;
#1521 = ORIENTED_EDGE ( 'NONE', *, *, #4504, .F. ) ;
#1522 = CARTESIAN_POINT ( 'NONE',  ( -47.94539818030330025, 150.5696653505793563, 0.000000000000000000 ) ) ;
#1523 =( GEOMETRIC_REPRESENTATION_CONTEXT ( 3 ) GLOBAL_UNCERTAINTY_ASSIGNED_CONTEXT ( ( #4366 ) ) GLOBAL_UNIT_ASSIGNED_CONTEXT ( ( #8417, #471, #3489 ) ) REPRESENTATION_CONTEXT ( 'NONE', 'WORKASPACE' ) );
#1524 = ORIENTED_EDGE ( 'NONE', *, *, #475, .F. ) ;
#1525 = APPLICATION_CONTEXT ( 'automotive_design' ) ;
#1526 = FACE_OUTER_BOUND ( 'NONE', #1367, .T. ) ;
#1527 =( NAMED_UNIT ( * ) SI_UNIT ( $, .STERADIAN. ) SOLID_ANGLE_UNIT ( ) );
#1528 = DIRECTION ( 'NONE',  ( 1.000000000000000000, 0.000000000000000000, 0.000000000000000000 ) ) ;
#1529 = ADVANCED_FACE ( 'NONE', ( #3007 ), #2321, .T. ) ;
#1530 = EDGE_CURVE ( 'NONE', #9884, #109, #7194, .T. ) ;
#1531 = DIRECTION ( 'NONE',  ( -0.6691306063588601249, -0.7431448254773928008, 0.000000000000000000 ) ) ;
#1532 = EDGE_CURVE ( 'NONE', #9083, #1931, #1954, .T. ) ;
#1533 = CARTESIAN_POINT ( 'NONE',  ( 14.70649310359190309, 120.5696653505793705, 16.00000000000000711 ) ) ;
#1534 = LINE ( 'NONE', #1625, #6676 ) ;
#1535 = VERTEX_POINT ( 'NONE', #7884 ) ;
#1536 = DIRECTION ( 'NONE',  ( -1.000000000000000000, -0.000000000000000000, -0.000000000000000000 ) ) ;
#1537 = ORIENTED_EDGE ( 'NONE', *, *, #7658, .T. ) ;
#1538 = LINE ( 'NONE', #5561, #7759 ) ;
#1539 = SURFACE_STYLE_FILL_AREA ( #6355 ) ;
#1540 = DIRECTION ( 'NONE',  ( -1.000000000000000000, -0.000000000000000000, -0.000000000000000000 ) ) ;
#1541 = LINE ( 'NONE', #3975, #3278 ) ;
#1542 = EDGE_CURVE ( 'NONE', #2621, #910, #1023, .T. ) ;
#1543 = DIRECTION ( 'NONE',  ( -0.9936146452197298640, 0.000000000000000000, -0.1128270216077272570 ) ) ;
#1544 = ORIENTED_EDGE ( 'NONE', *, *, #5654, .T. ) ;
#1545 = ORIENTED_EDGE ( 'NONE', *, *, #6642, .F. ) ;
#1546 = VECTOR ( 'NONE', #3114, 1000.000000000000000 ) ;
#1547 = ORIENTED_EDGE ( 'NONE', *, *, #2111, .F. ) ;
#1548 = CYLINDRICAL_SURFACE ( 'NONE', #5033, 4.999999999999997335 ) ;
#1549 = CARTESIAN_POINT ( 'NONE',  ( -24.98775663295400662, -134.6884760388430777, -50.00000000000001421 ) ) ;
#1550 = DIRECTION ( 'NONE',  ( -0.6691306063588565722, -0.7431448254773957984, 0.000000000000000000 ) ) ;
#1551 = ORIENTED_EDGE ( 'NONE', *, *, #6866, .F. ) ;
#1552 = AXIS2_PLACEMENT_3D ( 'NONE', #7863, #7967, #10359 ) ;
#1553 = CIRCLE ( 'NONE', #3938, 5.000000000000000888 ) ;
#1554 = EDGE_CURVE ( 'NONE', #10167, #5689, #1129, .T. ) ;
#1555 = EDGE_LOOP ( 'NONE', ( #6042, #8592, #8206, #858 ) ) ;
#1556 = ORIENTED_EDGE ( 'NONE', *, *, #6748, .F. ) ;
#1557 = DIRECTION ( 'NONE',  ( 1.000000000000000000, 1.277197683604454965E-16, -0.000000000000000000 ) ) ;
#1558 = SHAPE_REPRESENTATION_RELATIONSHIP ( 'NONE' , 'NONE' ,  #286, #5432 ) ;
#1559 = VECTOR ( 'NONE', #1130, 1000.000000000000000 ) ;
#1560 = AXIS2_PLACEMENT_3D ( 'NONE', #7664, #360, #6926 ) ;
#1561 = DIRECTION ( 'NONE',  ( 0.000000000000000000, 0.000000000000000000, 1.000000000000000000 ) ) ;
#1562 = CARTESIAN_POINT ( 'NONE',  ( 23.15769640663940265, -115.1457019118818863, -50.00000000000002132 ) ) ;
#1563 = VERTEX_POINT ( 'NONE', #8284 ) ;
#1564 = DIRECTION ( 'NONE',  ( -0.000000000000000000, 1.000000000000000000, -0.000000000000000000 ) ) ;
#1565 = ITEM_DEFINED_TRANSFORMATION ( 'NONE', 'NONE', #917,  #4601 ) ;
#1566 = EDGE_LOOP ( 'NONE', ( #5795, #7193, #8868, #923 ) ) ;
#1567 = AXIS2_PLACEMENT_3D ( 'NONE', #5827, #222, #9063 ) ;
#1568 = DIRECTION ( 'NONE',  ( 0.000000000000000000, 0.000000000000000000, 1.000000000000000000 ) ) ;
#1569 = ADVANCED_FACE ( 'NONE', ( #185 ), #5941, .F. ) ;
#1570 = EDGE_LOOP ( 'NONE', ( #231, #4645 ) ) ;
#1571 = ORIENTED_EDGE ( 'NONE', *, *, #634, .F. ) ;
#1572 = CARTESIAN_POINT ( 'NONE',  ( -40.00000000000002842, -135.1707019118818778, 35.99999999999998579 ) ) ;
#1573 = DIRECTION ( 'NONE',  ( 0.000000000000000000, -0.000000000000000000, -1.000000000000000000 ) ) ;
#1574 = EDGE_CURVE ( 'NONE', #1692, #8618, #4989, .T. ) ;
#1575 = CARTESIAN_POINT ( 'NONE',  ( 2.108096605167895612E-14, -115.1457019118818863, -25.15769640663941686 ) ) ;
#1576 = AXIS2_PLACEMENT_3D ( 'NONE', #2546, #119, #5722 ) ;
#1577 = DIRECTION ( 'NONE',  ( -0.000000000000000000, 0.000000000000000000, -1.000000000000000000 ) ) ;
#1578 = CYLINDRICAL_SURFACE ( 'NONE', #3499, 4.999999999999995559 ) ;
#1579 = ORIENTED_EDGE ( 'NONE', *, *, #554, .F. ) ;
#1580 = LINE ( 'NONE', #733, #9781 ) ;
#1581 = EDGE_CURVE ( 'NONE', #7949, #5630, #3311, .T. ) ;
#1582 = ADVANCED_FACE ( 'NONE', ( #9185 ), #971, .T. ) ;
#1583 = CIRCLE ( 'NONE', #3443, 4.000000000000007994 ) ;
#1584 = EDGE_CURVE ( 'NONE', #8, #5946, #776, .T. ) ;
#1585 = ORIENTED_EDGE ( 'NONE', *, *, #4551, .T. ) ;
#1586 = DIRECTION ( 'NONE',  ( -0.7431448254773957984, 0.6691306063588565722, -0.000000000000000000 ) ) ;
#1587 = CARTESIAN_POINT ( 'NONE',  ( -30.29350689640809335, 80.56966535057935630, -20.00000000000000711 ) ) ;
#1588 = CARTESIAN_POINT ( 'NONE',  ( -16.29350689640809691, 105.5289575273812233, -25.04213562373096380 ) ) ;
#1589 = CARTESIAN_POINT ( 'NONE',  ( -27.15769640663940976, -117.1457019118819005, 27.15769640663938489 ) ) ;
#1590 = ORIENTED_EDGE ( 'NONE', *, *, #3868, .F. ) ;
#1591 = CIRCLE ( 'NONE', #416, 5.000000000000000888 ) ;
#1592 = ORIENTED_EDGE ( 'NONE', *, *, #9396, .F. ) ;
#1593 = ORIENTED_EDGE ( 'NONE', *, *, #4957, .F. ) ;
#1594 = EDGE_CURVE ( 'NONE', #5925, #3441, #1074, .T. ) ;
#1595 = CARTESIAN_POINT ( 'NONE',  ( -50.00000000000002132, -133.1457019118818721, -23.15769640663945594 ) ) ;
#1596 = LINE ( 'NONE', #8757, #5448 ) ;
#1597 = AXIS2_PLACEMENT_3D ( 'NONE', #5049, #7006, #484 ) ;
#1598 = DIRECTION ( 'NONE',  ( -1.000000000000000000, -0.000000000000000000, -0.000000000000000000 ) ) ;
#1599 = DIRECTION ( 'NONE',  ( 1.000000000000000000, 0.000000000000000000, 0.000000000000000000 ) ) ;
#1600 = ORIENTED_EDGE ( 'NONE', *, *, #4252, .F. ) ;
#1601 = DIRECTION ( 'NONE',  ( -0.7431448254773957984, 0.6691306063588565722, -0.000000000000000000 ) ) ;
#1602 = ORIENTED_EDGE ( 'NONE', *, *, #2681, .T. ) ;
#1603 = SURFACE_SIDE_STYLE ('',( #4983 ) ) ;
#1604 = AXIS2_PLACEMENT_3D ( 'NONE', #9056, #7466, #9761 ) ;
#1605 = VERTEX_POINT ( 'NONE', #4307 ) ;
#1606 = AXIS2_PLACEMENT_3D ( 'NONE', #947, #4286, #1743 ) ;
#1607 = ORIENTED_EDGE ( 'NONE', *, *, #3884, .T. ) ;
#1608 = DIRECTION ( 'NONE',  ( 0.000000000000000000, 0.000000000000000000, -1.000000000000000000 ) ) ;
#1609 = DIRECTION ( 'NONE',  ( -1.000000000000000000, 0.000000000000000000, 0.000000000000000000 ) ) ;
#1610 = LINE ( 'NONE', #9729, #10068 ) ;
#1611 = ADVANCED_FACE ( 'NONE', ( #3517 ), #6691, .F. ) ;
#1612 = CARTESIAN_POINT ( 'NONE',  ( 37.29914372356918051, -134.6755117440382605, -25.86262238874442687 ) ) ;
#1613 = VERTEX_POINT ( 'NONE', #5839 ) ;
#1614 = CARTESIAN_POINT ( 'NONE',  ( 0.000000000000000000, -135.1457019118818721, 27.15769640663938489 ) ) ;
#1615 = ORIENTED_EDGE ( 'NONE', *, *, #3498, .T. ) ;
#1616 = CARTESIAN_POINT ( 'NONE',  ( -39.66851723004002395, -4.408728476930471151E-16, 3.600000000000004530 ) ) ;
#1617 = ORIENTED_EDGE ( 'NONE', *, *, #9294, .F. ) ;
#1618 = CIRCLE ( 'NONE', #7049, 0.4000000000000000222 ) ;
#1619 = EDGE_LOOP ( 'NONE', ( #5586, #3361, #7908, #7176 ) ) ;
#1620 = DIRECTION ( 'NONE',  ( -0.7431448254773957984, 0.6691306063588565722, -0.000000000000000000 ) ) ;
#1621 = DIRECTION ( 'NONE',  ( -0.000000000000000000, -0.000000000000000000, -1.000000000000000000 ) ) ;
#1622 = CARTESIAN_POINT ( 'NONE',  ( -48.00000000000002132, -135.1457019118818721, 25.15769640663938134 ) ) ;
#1623 = VECTOR ( 'NONE', #5440, 1000.000000000000000 ) ;
#1624 = CARTESIAN_POINT ( 'NONE',  ( -7.293506896408097795, -3.651280424770854409E-15, 24.99999999999998579 ) ) ;
#1625 = CARTESIAN_POINT ( 'NONE',  ( 25.15769640663937778, -117.1457019118819005, -25.15769640663940976 ) ) ;
#1626 = PRODUCT_DEFINITION_SHAPE ( 'NONE', 'NONE',  #10487 ) ;
#1627 = EDGE_CURVE ( 'NONE', #8144, #9162, #5733, .T. ) ;
#1628 = VECTOR ( 'NONE', #1716, 1000.000000000000000 ) ;
#1629 = ORIENTED_EDGE ( 'NONE', *, *, #8965, .F. ) ;
#1630 = CARTESIAN_POINT ( 'NONE',  ( -27.85255513972543895, 150.5696653505793563, 7.750000000000002665 ) ) ;
#1631 = VECTOR ( 'NONE', #6051, 1000.000000000000000 ) ;
#1632 = EDGE_LOOP ( 'NONE', ( #2607, #2789, #4830, #9276, #8779, #2786, #443, #7436, #10424, #10141, #9748, #952, #4956, #10358, #2505, #2868, #10031, #8560, #156, #3347 ) ) ;
#1633 = DIRECTION ( 'NONE',  ( 0.000000000000000000, 0.000000000000000000, 1.000000000000000000 ) ) ;
#1634 = DIRECTION ( 'NONE',  ( -0.000000000000000000, -0.000000000000000000, -1.000000000000000000 ) ) ;
#1635 = AXIS2_PLACEMENT_3D ( 'NONE', #2392, #3294, #6585 ) ;
#1636 = CARTESIAN_POINT ( 'NONE',  ( 38.19229777560031636, 118.3760186273086816, 30.00000000000000355 ) ) ;
#1637 = LINE ( 'NONE', #1796, #4788 ) ;
#1638 = DIRECTION ( 'NONE',  ( -0.6691306063588564612, -0.7431448254773956874, 0.000000000000000000 ) ) ;
#1639 = DIRECTION ( 'NONE',  ( 1.000000000000000000, 0.000000000000000000, 6.982941293900099513E-16 ) ) ;
#1640 = EDGE_LOOP ( 'NONE', ( #4239, #7288, #2353 ) ) ;
#1641 = EDGE_CURVE ( 'NONE', #1403, #5730, #6745, .T. ) ;
#1642 = VECTOR ( 'NONE', #6073, 1000.000000000000000 ) ;
#1643 = EDGE_CURVE ( 'NONE', #4089, #6869, #3464, .T. ) ;
#1644 = VERTEX_POINT ( 'NONE', #9993 ) ;
#1645 = ORIENTED_EDGE ( 'NONE', *, *, #8978, .F. ) ;
#1646 = VECTOR ( 'NONE', #7816, 1000.000000000000000 ) ;
#1647 = ORIENTED_EDGE ( 'NONE', *, *, #7, .F. ) ;
#1648 = LINE ( 'NONE', #3394, #2167 ) ;
#1649 = DIRECTION ( 'NONE',  ( -0.000000000000000000, 0.000000000000000000, 1.000000000000000000 ) ) ;
#1650 = CLOSED_SHELL ( 'NONE', ( #7791, #3659, #9210, #212, #5565, #7031, #9427, #3445, #2066, #4946, #1859, #4633, #90, #558, #8713, #9425, #9166, #8376, #7968, #2461, #345, #3557, #7629, #1397, #2302, #4694, #4269 ) ) ;
#1651 = LINE ( 'NONE', #6320, #5962 ) ;
#1652 = AXIS2_PLACEMENT_3D ( 'NONE', #1809, #7430, #9122 ) ;
#1653 = ORIENTED_EDGE ( 'NONE', *, *, #1641, .T. ) ;
#1654 = ADVANCED_FACE ( 'NONE', ( #1920 ), #3363, .F. ) ;
#1655 = DIRECTION ( 'NONE',  ( -0.7431448254773957984, 0.6691306063588565722, -0.000000000000000000 ) ) ;
#1656 = EDGE_CURVE ( 'NONE', #2182, #847, #9132, .T. ) ;
#1657 = ADVANCED_FACE ( 'NONE', ( #2713 ), #8398, .T. ) ;
#1658 = VERTEX_POINT ( 'NONE', #5152 ) ;
#1659 =( NAMED_UNIT ( * ) PLANE_ANGLE_UNIT ( ) SI_UNIT ( $, .RADIAN. ) );
#1660 = CIRCLE ( 'NONE', #7585, 4.025000000000000355 ) ;
#1661 =( REPRESENTATION_RELATIONSHIP ('NONE','NONE', #9007, #7587 ) REPRESENTATION_RELATIONSHIP_WITH_TRANSFORMATION ( #6650 )SHAPE_REPRESENTATION_RELATIONSHIP( ) );
#1662 = ORIENTED_EDGE ( 'NONE', *, *, #7675, .T. ) ;
#1663 = CARTESIAN_POINT ( 'NONE',  ( -45.00000000000000000, 0.4000000000000000222, 0.000000000000000000 ) ) ;
#1664 = CARTESIAN_POINT ( 'NONE',  ( 0.000000000000000000, -135.1457019118818721, 30.00000000000000355 ) ) ;
#1665 = CARTESIAN_POINT ( 'NONE',  ( -16.29350689640809691, -8.660287962196477451, 5.025000000000002132 ) ) ;
#1666 = VECTOR ( 'NONE', #2803, 1000.000000000000000 ) ;
#1667 = DIRECTION ( 'NONE',  ( 1.000000000000000000, 0.000000000000000000, -1.137729606058012035E-16 ) ) ;
#1668 = LINE ( 'NONE', #188, #113 ) ;
#1669 = EDGE_CURVE ( 'NONE', #2192, #195, #5789, .T. ) ;
#1670 = VERTEX_POINT ( 'NONE', #9028 ) ;
#1671 = DIRECTION ( 'NONE',  ( 0.000000000000000000, 1.000000000000000000, 0.000000000000000000 ) ) ;
#1672 = ORIENTED_EDGE ( 'NONE', *, *, #105, .F. ) ;
#1673 = CARTESIAN_POINT ( 'NONE',  ( -25.93999053166054480, -135.0799163051958942, 49.99999999999999289 ) ) ;
#1674 = ORIENTED_EDGE ( 'NONE', *, *, #9568, .F. ) ;
#1675 = EDGE_CURVE ( 'NONE', #10069, #2784, #1393, .T. ) ;
#1676 = DIRECTION ( 'NONE',  ( -1.000000000000000000, 0.000000000000000000, 0.000000000000000000 ) ) ;
#1677 = LINE ( 'NONE', #4849, #5306 ) ;
#1678 = DIRECTION ( 'NONE',  ( -0.5150380749100536004, 1.049727191138618942E-16, -0.8571673007021125557 ) ) ;
#1679 = CARTESIAN_POINT ( 'NONE',  ( 27.15769640663936713, -135.1457019118818721, 27.15769640663938489 ) ) ;
#1680 = SPHERICAL_SURFACE ( 'NONE', #2071, 8.000000000000000000 ) ;
#1681 = ORIENTED_EDGE ( 'NONE', *, *, #846, .T. ) ;
#1682 = DIRECTION ( 'NONE',  ( -1.000000000000000000, 0.000000000000000000, 0.000000000000000000 ) ) ;
#1683 = EDGE_CURVE ( 'NONE', #1083, #1913, #4521, .T. ) ;
#1684 = EDGE_LOOP ( 'NONE', ( #3521, #4698 ) ) ;
#1685 = CARTESIAN_POINT ( 'NONE',  ( -16.29350689640809691, 105.5289575273812233, 7.750000000000000000 ) ) ;
#1686 = DIRECTION ( 'NONE',  ( 0.000000000000000000, 1.000000000000000000, -1.460512169908342690E-16 ) ) ;
#1687 = EDGE_CURVE ( 'NONE', #6849, #5630, #2077, .T. ) ;
#1688 =( LENGTH_UNIT ( ) NAMED_UNIT ( * ) SI_UNIT ( .MILLI., .METRE. ) );
#1689 = DIRECTION ( 'NONE',  ( -0.000000000000000000, -0.000000000000000000, 1.000000000000000000 ) ) ;
#1690 = CARTESIAN_POINT ( 'NONE',  ( 0.000000000000000000, -117.1457019118819005, 23.15769640663938134 ) ) ;
#1691 = CARTESIAN_POINT ( 'NONE',  ( -7.293506896408105789, 150.5696653505793563, -20.00000000000000355 ) ) ;
#1692 = VERTEX_POINT ( 'NONE', #5416 ) ;
#1693 = EDGE_LOOP ( 'NONE', ( #5685, #1938, #1873 ) ) ;
#1694 = EDGE_LOOP ( 'NONE', ( #5212, #3936, #7368, #49 ) ) ;
#1695 = VERTEX_POINT ( 'NONE', #7756 ) ;
#1696 = EDGE_CURVE ( 'NONE', #6030, #4567, #3781, .T. ) ;
#1697 = LINE ( 'NONE', #8319, #3178 ) ;
#1698 = DIRECTION ( 'NONE',  ( 1.000000000000000000, 0.000000000000000000, 0.000000000000000000 ) ) ;
#1699 = DIRECTION ( 'NONE',  ( 0.000000000000000000, 0.000000000000000000, 1.000000000000000000 ) ) ;
#1700 = LINE ( 'NONE', #1013, #639 ) ;
#1701 = ORIENTED_EDGE ( 'NONE', *, *, #10367, .F. ) ;
#1702 = CARTESIAN_POINT ( 'NONE',  ( -142.3328939341254795, 249.4204141414382434, 0.000000000000000000 ) ) ;
#1703 = ORIENTED_EDGE ( 'NONE', *, *, #6039, .T. ) ;
#1704 = CARTESIAN_POINT ( 'NONE',  ( -8.000000000000000000, 0.1799657291978528917, -2.057017697435775005 ) ) ;
#1705 = EDGE_LOOP ( 'NONE', ( #2413, #6183, #5141, #2782, #6435, #883, #5365 ) ) ;
#1706 = CIRCLE ( 'NONE', #8135, 7.999999999999991118 ) ;
#1707 = EDGE_CURVE ( 'NONE', #2362, #6151, #617, .T. ) ;
#1708 = DIRECTION ( 'NONE',  ( -1.000000000000000000, 0.000000000000000000, 1.137729606058012035E-16 ) ) ;
#1709 = EDGE_CURVE ( 'NONE', #5357, #9948, #9345, .T. ) ;
#1710 = DIRECTION ( 'NONE',  ( -0.000000000000000000, -0.000000000000000000, 1.000000000000000000 ) ) ;
#1711 = EDGE_CURVE ( 'NONE', #5823, #5289, #7017, .T. ) ;
#1712 = CARTESIAN_POINT ( 'NONE',  ( -39.00428932080996702, 3.095342794014916965, -1.752073144804183080 ) ) ;
#1713 = DIRECTION ( 'NONE',  ( -1.000000000000000000, 0.000000000000000000, 1.396588258780020149E-16 ) ) ;
#1714 = PRODUCT_DEFINITION_SHAPE ( 'NONE', 'NONE',  #10489 ) ;
#1715 = DIRECTION ( 'NONE',  ( 1.000000000000000000, 0.000000000000000000, 0.000000000000000000 ) ) ;
#1716 = DIRECTION ( 'NONE',  ( 0.000000000000000000, 0.7071067811864494290, 0.7071067811866454944 ) ) ;
#1717 = VECTOR ( 'NONE', #85, 1000.000000000000000 ) ;
#1718 = ORIENTED_EDGE ( 'NONE', *, *, #9977, .F. ) ;
#1719 = VECTOR ( 'NONE', #6591, 1000.000000000000000 ) ;
#1720 = DIRECTION ( 'NONE',  ( -0.000000000000000000, 1.000000000000000000, -0.000000000000000000 ) ) ;
#1721 = ITEM_DEFINED_TRANSFORMATION ( 'NONE', 'NONE', #10234,  #4601 ) ;
#1722 = VERTEX_POINT ( 'NONE', #7700 ) ;
#1723 = PLANE ( 'NONE',  #825 ) ;
#1724 = ORIENTED_EDGE ( 'NONE', *, *, #8711, .T. ) ;
#1725 = CIRCLE ( 'NONE', #10190, 2.000000000000001776 ) ;
#1726 = ADVANCED_FACE ( 'NONE', ( #10036 ), #446, .F. ) ;
#1727 = AXIS2_PLACEMENT_3D ( 'NONE', #6580, #1649, #1698 ) ;
#1728 = DIRECTION ( 'NONE',  ( -1.000000000000000000, 0.000000000000000000, 0.000000000000000000 ) ) ;
#1729 = CARTESIAN_POINT ( 'NONE',  ( -8.793506896408096907, 120.5289575273812233, -7.750000000000000000 ) ) ;
#1730 = DIRECTION ( 'NONE',  ( -1.000000000000000000, -0.000000000000000000, -0.000000000000000000 ) ) ;
#1731 = FILL_AREA_STYLE ('',( #8992 ) ) ;
#1732 = FACE_OUTER_BOUND ( 'NONE', #6195, .T. ) ;
#1733 = AXIS2_PLACEMENT_3D ( 'NONE', #7041, #8623, #6238 ) ;
#1734 = AXIS2_PLACEMENT_3D ( 'NONE', #8821, #10265, #8024 ) ;
#1735 = ORIENTED_EDGE ( 'NONE', *, *, #5397, .F. ) ;
#1736 = CARTESIAN_POINT ( 'NONE',  ( -30.29350689640809335, -0.3998014571812398832, -1.076388538564875708 ) ) ;
#1737 = ORIENTED_EDGE ( 'NONE', *, *, #354, .F. ) ;
#1738 = LINE ( 'NONE', #4127, #5048 ) ;
#1739 = AXIS2_PLACEMENT_3D ( 'NONE', #2928, #9239, #10092 ) ;
#1740 = LINE ( 'NONE', #1636, #7953 ) ;
#1741 = CARTESIAN_POINT ( 'NONE',  ( -23.15769640663940976, -135.1457019118818721, 47.99999999999997868 ) ) ;
#1742 = AXIS2_PLACEMENT_3D ( 'NONE', #4654, #5446, #6243 ) ;
#1743 = DIRECTION ( 'NONE',  ( -1.000000000000000000, 0.000000000000000000, 0.000000000000000000 ) ) ;
#1744 = CARTESIAN_POINT ( 'NONE',  ( -20.29350689640810401, 150.5696653505793563, -10.98204862120179826 ) ) ;
#1745 = ADVANCED_FACE ( 'NONE', ( #9238 ), #6205, .F. ) ;
#1746 = VERTEX_POINT ( 'NONE', #10143 ) ;
#1747 = EDGE_LOOP ( 'NONE', ( #1592, #5328, #555, #6139, #7007, #1929 ) ) ;
#1748 = AXIS2_PLACEMENT_3D ( 'NONE', #3396, #6681, #1860 ) ;
#1749 = ORIENTED_EDGE ( 'NONE', *, *, #10145, .T. ) ;
#1750 = DIRECTION ( 'NONE',  ( -1.387778780781445676E-16, 0.000000000000000000, 1.000000000000000000 ) ) ;
#1751 = CARTESIAN_POINT ( 'NONE',  ( 37.22759939293836595, -117.1457019118819005, -25.15769640663939910 ) ) ;
#1752 = DIRECTION ( 'NONE',  ( 1.000000000000000000, 0.000000000000000000, 0.000000000000000000 ) ) ;
#1753 = CARTESIAN_POINT ( 'NONE',  ( -2.293506896408094242, 37.08684478514405214, 12.50000000000000000 ) ) ;
#1754 = TOROIDAL_SURFACE ( 'NONE', #7008, 75.59748767972220662, 70.74985237403969052 ) ;
#1755 = ORIENTED_EDGE ( 'NONE', *, *, #8260, .T. ) ;
#1756 = CARTESIAN_POINT ( 'NONE',  ( 37.22759939293836595, -117.1457019118819005, -25.15769640663939910 ) ) ;
#1757 = EDGE_LOOP ( 'NONE', ( #4011, #652, #8539, #8069 ) ) ;
#1758 = DIRECTION ( 'NONE',  ( -0.7431448254773957984, 0.6691306063588565722, -0.000000000000000000 ) ) ;
#1759 = ADVANCED_FACE ( 'NONE', ( #546 ), #9295, .F. ) ;
#1760 = AXIS2_PLACEMENT_3D ( 'NONE', #680, #3111, #2163 ) ;
#1761 = ORIENTED_EDGE ( 'NONE', *, *, #7993, .T. ) ;
#1762 = UNCERTAINTY_MEASURE_WITH_UNIT (LENGTH_MEASURE( 1.000000000000000082E-05 ), #9279, 'distance_accuracy_value', 'NONE');
#1763 = DIRECTION ( 'NONE',  ( 0.000000000000000000, 0.000000000000000000, 1.000000000000000000 ) ) ;
#1764 =( LENGTH_UNIT ( ) NAMED_UNIT ( * ) SI_UNIT ( .MILLI., .METRE. ) );
#1765 = CARTESIAN_POINT ( 'NONE',  ( 10.26554134690924691, 150.5696653505793563, -7.750000000000000000 ) ) ;
#1766 = DIRECTION ( 'NONE',  ( 0.000000000000000000, 0.000000000000000000, 1.000000000000000000 ) ) ;
#1767 = DIRECTION ( 'NONE',  ( -8.194486552889013533E-17, -9.100899318238110877E-17, 1.000000000000000000 ) ) ;
#1768 = DIRECTION ( 'NONE',  ( 0.000000000000000000, 0.000000000000000000, -1.000000000000000000 ) ) ;
#1769 = VECTOR ( 'NONE', #2995, 1000.000000000000000 ) ;
#1770 = ORIENTED_EDGE ( 'NONE', *, *, #1110, .T. ) ;
#1771 = CARTESIAN_POINT ( 'NONE',  ( -24.31850689640809549, 140.5696653505793563, -7.749999999999996447 ) ) ;
#1772 = EDGE_CURVE ( 'NONE', #510, #4261, #8231, .T. ) ;
#1773 = ADVANCED_FACE ( 'NONE', ( #8650 ), #1344, .F. ) ;
#1774 = EDGE_CURVE ( 'NONE', #5946, #8972, #6214, .T. ) ;
#1775 = APPLICATION_PROTOCOL_DEFINITION ( 'draft international standard', 'automotive_design', 1998, #8151 ) ;
#1776 = ORIENTED_EDGE ( 'NONE', *, *, #6748, .T. ) ;
#1777 = CARTESIAN_POINT ( 'NONE',  ( 27.15769640663940621, -133.1457019118818721, -48.00000000000002132 ) ) ;
#1778 = ORIENTED_EDGE ( 'NONE', *, *, #3266, .T. ) ;
#1779 = VECTOR ( 'NONE', #9160, 1000.000000000000000 ) ;
#1780 = CARTESIAN_POINT ( 'NONE',  ( 27.15769640663938489, -133.1457019118818721, -27.15769640663940976 ) ) ;
#1781 = CARTESIAN_POINT ( 'NONE',  ( -16.29350689640809691, -7.660287962196459688, 0.000000000000000000 ) ) ;
#1782 = DIRECTION ( 'NONE',  ( 0.000000000000000000, 0.000000000000000000, -1.000000000000000000 ) ) ;
#1783 = DIRECTION ( 'NONE',  ( 0.000000000000000000, 0.000000000000000000, -1.000000000000000000 ) ) ;
#1784 = FACE_OUTER_BOUND ( 'NONE', #6548, .T. ) ;
#1785 = PRODUCT_DEFINITION ( 'UNKNOWN', '', #7350, #6637 ) ;
#1786 = EDGE_CURVE ( 'NONE', #954, #9488, #2649, .T. ) ;
#1787 = EDGE_CURVE ( 'NONE', #2404, #9616, #2988, .T. ) ;
#1788 = EDGE_LOOP ( 'NONE', ( #8956, #7525, #5665, #603 ) ) ;
#1789 = AXIS2_PLACEMENT_3D ( 'NONE', #9467, #7818, #715 ) ;
#1790 = CARTESIAN_POINT ( 'NONE',  ( 25.15769640663936713, -133.1457019118818721, 47.99999999999997868 ) ) ;
#1791 = ORIENTED_EDGE ( 'NONE', *, *, #4447, .F. ) ;
#1792 = LINE ( 'NONE', #4859, #8780 ) ;
#1793 = CARTESIAN_POINT ( 'NONE',  ( -7.293506896408097795, -3.651280424770854409E-15, -24.99999999999998579 ) ) ;
#1794 = AXIS2_PLACEMENT_3D ( 'NONE', #293, #4256, #3409 ) ;
#1795 = CARTESIAN_POINT ( 'NONE',  ( -40.00000000000002842, -115.1457019118818863, 49.99999999999997868 ) ) ;
#1796 = CARTESIAN_POINT ( 'NONE',  ( -7.293506896408097795, 72.08684478514406635, 28.00000000000001066 ) ) ;
#1797 = LINE ( 'NONE', #56, #10081 ) ;
#1798 = PLANE ( 'NONE',  #3297 ) ;
#1799 = EDGE_CURVE ( 'NONE', #2463, #4407, #3321, .T. ) ;
#1800 = VERTEX_POINT ( 'NONE', #4571 ) ;
#1801 = ORIENTED_EDGE ( 'NONE', *, *, #3926, .T. ) ;
#1802 = VECTOR ( 'NONE', #5450, 1000.000000000000000 ) ;
#1803 = AXIS2_PLACEMENT_3D ( 'NONE', #5143, #9067, #3562 ) ;
#1804 = ORIENTED_EDGE ( 'NONE', *, *, #7866, .F. ) ;
#1805 = LINE ( 'NONE', #9013, #4531 ) ;
#1806 = ADVANCED_FACE ( 'NONE', ( #3623 ), #10091, .T. ) ;
#1807 = CARTESIAN_POINT ( 'NONE',  ( 33.55285093437175448, 29.14909237014565946, 30.00000000000000355 ) ) ;
#1808 = DIRECTION ( 'NONE',  ( 0.000000000000000000, 0.000000000000000000, 1.000000000000000000 ) ) ;
#1809 = CARTESIAN_POINT ( 'NONE',  ( 6.250000000000005329, 0.000000000000000000, -3.250000000000000444 ) ) ;
#1810 = VECTOR ( 'NONE', #2046, 1000.000000000000000 ) ;
#1811 = VERTEX_POINT ( 'NONE', #4822 ) ;
#1812 = LINE ( 'NONE', #6786, #2141 ) ;
#1813 = ORIENTED_EDGE ( 'NONE', *, *, #2108, .F. ) ;
#1814 = AXIS2_PLACEMENT_3D ( 'NONE', #1142, #1088, #6757 ) ;
#1815 = FILL_AREA_STYLE ('',( #4200 ) ) ;
#1816 = VERTEX_POINT ( 'NONE', #10355 ) ;
#1817 = LINE ( 'NONE', #6590, #2828 ) ;
#1818 = VECTOR ( 'NONE', #8221, 1000.000000000000114 ) ;
#1819 = CARTESIAN_POINT ( 'NONE',  ( -7.293506896408097795, 2.445795361565304815E-15, -20.00000000000002132 ) ) ;
#1820 = CARTESIAN_POINT ( 'NONE',  ( 3.000000000000000000, -1.467624384280032279, -2.541999999999998039 ) ) ;
#1821 = DIRECTION ( 'NONE',  ( -0.7431448254773957984, 0.6691306063588565722, -0.000000000000000000 ) ) ;
#1822 = CARTESIAN_POINT ( 'NONE',  ( -153.9940972124336156, 259.9202087346060921, 0.000000000000000000 ) ) ;
#1823 = AXIS2_PLACEMENT_3D ( 'NONE', #234, #3460, #4885 ) ;
#1824 = ORIENTED_EDGE ( 'NONE', *, *, #2233, .T. ) ;
#1825 = DIRECTION ( 'NONE',  ( -1.000000000000000000, 0.000000000000000000, 0.000000000000000000 ) ) ;
#1826 = CONICAL_SURFACE ( 'NONE', #6683, 4.025000000000000355, 0.7853981633975870569 ) ;
#1827 = ORIENTED_EDGE ( 'NONE', *, *, #4004, .T. ) ;
#1828 = FACE_OUTER_BOUND ( 'NONE', #10076, .T. ) ;
#1829 = ORIENTED_EDGE ( 'NONE', *, *, #9438, .T. ) ;
#1830 = AXIS2_PLACEMENT_3D ( 'NONE', #3609, #9278, #9979 ) ;
#1831 = EDGE_CURVE ( 'NONE', #4261, #596, #7858, .T. ) ;
#1832 = SPHERICAL_SURFACE ( 'NONE', #632, 8.000000000000000000 ) ;
#1833 = CARTESIAN_POINT ( 'NONE',  ( 3.000000000000000000, 2.935248768560057897, -3.252606517456513302E-15 ) ) ;
#1834 = CARTESIAN_POINT ( 'NONE',  ( -23.79350689640809691, 120.5289575273812233, 54.43095569077609497 ) ) ;
#1835 = FACE_OUTER_BOUND ( 'NONE', #7369, .T. ) ;
#1836 = LINE ( 'NONE', #6554, #3429 ) ;
#1837 = AXIS2_PLACEMENT_3D ( 'NONE', #5705, #6667, #1633 ) ;
#1838 = ORIENTED_EDGE ( 'NONE', *, *, #2430, .T. ) ;
#1839 = CARTESIAN_POINT ( 'NONE',  ( -148.5890485138274357, 243.3411686721859724, 0.000000000000000000 ) ) ;
#1840 =( GEOMETRIC_REPRESENTATION_CONTEXT ( 3 ) GLOBAL_UNCERTAINTY_ASSIGNED_CONTEXT ( ( #5531 ) ) GLOBAL_UNIT_ASSIGNED_CONTEXT ( ( #7330, #1659, #3296 ) ) REPRESENTATION_CONTEXT ( 'NONE', 'WORKASPACE' ) );
#1841 = ORIENTED_EDGE ( 'NONE', *, *, #10189, .F. ) ;
#1842 = DIRECTION ( 'NONE',  ( 1.000000000000000000, -0.000000000000000000, -1.137729606058012035E-16 ) ) ;
#1843 = EDGE_CURVE ( 'NONE', #8639, #4912, #3087, .T. ) ;
#1844 = CARTESIAN_POINT ( 'NONE',  ( -30.29350689640809335, 50.54838324668256888, 20.00000000000001776 ) ) ;
#1845 = ADVANCED_FACE ( 'NONE', ( #4726 ), #8704, .F. ) ;
#1846 = EDGE_CURVE ( 'NONE', #4360, #2186, #6492, .T. ) ;
#1847 = LINE ( 'NONE', #1795, #5904 ) ;
#1848 = CARTESIAN_POINT ( 'NONE',  ( -16.29350689640809691, -145.1457019118819005, 0.000000000000000000 ) ) ;
#1849 = DIRECTION ( 'NONE',  ( 1.000000000000000000, 0.000000000000000000, -0.000000000000000000 ) ) ;
#1850 = CARTESIAN_POINT ( 'NONE',  ( 3.000000000000000000, -1.467624384280024730, 2.542000000000003368 ) ) ;
#1851 = VECTOR ( 'NONE', #9375, 1000.000000000000000 ) ;
#1852 = EDGE_LOOP ( 'NONE', ( #897, #1347, #7000, #8533, #3240, #6980, #4738, #1854 ) ) ;
#1853 = ORIENTED_EDGE ( 'NONE', *, *, #4817, .T. ) ;
#1854 = ORIENTED_EDGE ( 'NONE', *, *, #8258, .T. ) ;
#1855 = CIRCLE ( 'NONE', #3209, 4.000000000000000000 ) ;
#1856 = CARTESIAN_POINT ( 'NONE',  ( -38.96131932220313132, 0.2735269159956709717, 3.990636919869543942 ) ) ;
#1857 = DIRECTION ( 'NONE',  ( 0.000000000000000000, 1.000000000000000000, 0.000000000000000000 ) ) ;
#1858 =( REPRESENTATION_RELATIONSHIP ('NONE','NONE', #9007, #6905 ) REPRESENTATION_RELATIONSHIP_WITH_TRANSFORMATION ( #3418 )SHAPE_REPRESENTATION_RELATIONSHIP( ) );
#1859 = ADVANCED_FACE ( 'NONE', ( #2242 ), #4679, .T. ) ;
#1860 = DIRECTION ( 'NONE',  ( 0.000000000000000000, 0.000000000000000000, 1.000000000000000000 ) ) ;
#1861 = CYLINDRICAL_SURFACE ( 'NONE', #8080, 4.000000000000000000 ) ;
#1862 = EDGE_LOOP ( 'NONE', ( #8414, #8544, #3619, #7668, #2073, #193 ) ) ;
#1863 = CARTESIAN_POINT ( 'NONE',  ( -166.0794662972351716, 270.8019239353934040, 0.000000000000000000 ) ) ;
#1864 = EDGE_LOOP ( 'NONE', ( #4693, #2674, #4241, #1507, #2287, #1672 ) ) ;
#1865 = CARTESIAN_POINT ( 'NONE',  ( 3.000000000000000000, 0.000000000000000000, 0.000000000000000000 ) ) ;
#1866 = ORIENTED_EDGE ( 'NONE', *, *, #5218, .F. ) ;
#1867 = DIRECTION ( 'NONE',  ( 0.000000000000000000, 0.000000000000000000, -1.000000000000000000 ) ) ;
#1868 = CARTESIAN_POINT ( 'NONE',  ( 18.34874108452142494, -140.1746510883711778, -97.78965767959371647 ) ) ;
#1869 = DIRECTION ( 'NONE',  ( -0.000000000000000000, 1.000000000000000000, -0.000000000000000000 ) ) ;
#1870 = CARTESIAN_POINT ( 'NONE',  ( -2.293506896408097795, 145.5696653505793563, 20.00000000000000711 ) ) ;
#1871 = CARTESIAN_POINT ( 'NONE',  ( -24.29350689640808980, 140.5696653505793563, 19.97500000000000853 ) ) ;
#1872 = CYLINDRICAL_SURFACE ( 'NONE', #10436, 4.729641367753004033 ) ;
#1873 = ORIENTED_EDGE ( 'NONE', *, *, #1973, .T. ) ;
#1874 = EDGE_CURVE ( 'NONE', #581, #2404, #7071, .T. ) ;
#1875 = CARTESIAN_POINT ( 'NONE',  ( 18.34874108452142494, -140.1746510883711778, -50.00000000000002132 ) ) ;
#1876 = EDGE_CURVE ( 'NONE', #2362, #4450, #4513, .T. ) ;
#1877 = CIRCLE ( 'NONE', #6619, 3.250000000000000444 ) ;
#1878 = ORIENTED_EDGE ( 'NONE', *, *, #804, .F. ) ;
#1879 = FACE_OUTER_BOUND ( 'NONE', #967, .T. ) ;
#1880 = ORIENTED_EDGE ( 'NONE', *, *, #6629, .F. ) ;
#1881 = CIRCLE ( 'NONE', #54, 24.00000000000002132 ) ;
#1882 = CARTESIAN_POINT ( 'NONE',  ( 37.22511195853869026, -145.1457019118819005, 30.00000000000000355 ) ) ;
#1883 = CIRCLE ( 'NONE', #5264, 5.000000000000000888 ) ;
#1884 = CARTESIAN_POINT ( 'NONE',  ( 37.60382362833208703, -135.1346843322565121, 26.91340685820611611 ) ) ;
#1885 = CARTESIAN_POINT ( 'NONE',  ( 0.000000000000000000, -1.467624384280024730, 2.542000000000003368 ) ) ;
#1886 = VERTEX_POINT ( 'NONE', #10456 ) ;
#1887 = FACE_OUTER_BOUND ( 'NONE', #8797, .T. ) ;
#1888 = EDGE_CURVE ( 'NONE', #822, #7959, #6023, .T. ) ;
#1889 = VERTEX_POINT ( 'NONE', #3894 ) ;
#1890 = DIRECTION ( 'NONE',  ( 0.000000000000000000, 0.000000000000000000, 1.000000000000000000 ) ) ;
#1891 = ORIENTED_EDGE ( 'NONE', *, *, #856, .T. ) ;
#1892 = CYLINDRICAL_SURFACE ( 'NONE', #8905, 2.000000000000001776 ) ;
#1893 = CARTESIAN_POINT ( 'NONE',  ( 0.000000000000000000, -115.1457019118818863, 25.15769640663938134 ) ) ;
#1894 = DIRECTION ( 'NONE',  ( -1.000000000000000000, 0.000000000000000000, 0.000000000000000000 ) ) ;
#1895 = DIRECTION ( 'NONE',  ( -0.000000000000000000, 0.8660254037844394848, 0.4999999999999985567 ) ) ;
#1896 = CARTESIAN_POINT ( 'NONE',  ( -45.00000000000000000, -0.4000000000000000222, -2.694222958124179965E-16 ) ) ;
#1897 = VECTOR ( 'NONE', #9971, 1000.000000000000000 ) ;
#1898 = DIRECTION ( 'NONE',  ( 1.000000000000000000, 0.000000000000000000, 0.000000000000000000 ) ) ;
#1899 = AXIS2_PLACEMENT_3D ( 'NONE', #7238, #3907, #6336 ) ;
#1900 = ORIENTED_EDGE ( 'NONE', *, *, #4631, .T. ) ;
#1901 = ADVANCED_FACE ( 'NONE', ( #2389 ), #7124, .F. ) ;
#1902 = EDGE_CURVE ( 'NONE', #2551, #1535, #6369, .T. ) ;
#1903 = VERTEX_POINT ( 'NONE', #1502 ) ;
#1904 = EDGE_CURVE ( 'NONE', #1658, #5357, #701, .T. ) ;
#1905 = CIRCLE ( 'NONE', #1739, 1.999999999999998224 ) ;
#1906 = VECTOR ( 'NONE', #5257, 1000.000000000000000 ) ;
#1907 = LINE ( 'NONE', #3556, #9287 ) ;
#1908 = DIRECTION ( 'NONE',  ( -0.7431448254773957984, 0.6691306063588564612, 0.000000000000000000 ) ) ;
#1909 = DIRECTION ( 'NONE',  ( 0.000000000000000000, 0.000000000000000000, 1.000000000000000000 ) ) ;
#1910 = EDGE_LOOP ( 'NONE', ( #8695, #8822, #1055, #10301, #9500, #114, #7753, #6264 ) ) ;
#1911 = FACE_OUTER_BOUND ( 'NONE', #1175, .T. ) ;
#1912 = VECTOR ( 'NONE', #8848, 1000.000000000000000 ) ;
#1913 = VERTEX_POINT ( 'NONE', #7172 ) ;
#1914 = CARTESIAN_POINT ( 'NONE',  ( -40.00000000000002842, -135.1707019118818778, 43.99999999999997868 ) ) ;
#1915 = EDGE_CURVE ( 'NONE', #4722, #581, #3259, .T. ) ;
#1916 = EDGE_LOOP ( 'NONE', ( #3525, #7798, #9101, #10095 ) ) ;
#1917 = CARTESIAN_POINT ( 'NONE',  ( -117.0000000000000000, 3.319229491889298167, -2.232199717805803729 ) ) ;
#1918 = DIRECTION ( 'NONE',  ( 0.000000000000000000, 0.000000000000000000, -1.000000000000000000 ) ) ;
#1919 = AXIS2_PLACEMENT_3D ( 'NONE', #2644, #9706, #211 ) ;
#1920 = FACE_OUTER_BOUND ( 'NONE', #3172, .T. ) ;
#1921 = CARTESIAN_POINT ( 'NONE',  ( -23.76520584195948516, -145.1457019118819005, -50.00000000000002132 ) ) ;
#1922 = VECTOR ( 'NONE', #3126, 1000.000000000000000 ) ;
#1923 = DIRECTION ( 'NONE',  ( 1.000000000000000000, 0.000000000000000000, 0.000000000000000000 ) ) ;
#1924 = DIRECTION ( 'NONE',  ( -1.000000000000000000, -0.000000000000000000, -0.000000000000000000 ) ) ;
#1925 = ORIENTED_EDGE ( 'NONE', *, *, #7233, .F. ) ;
#1926 = CARTESIAN_POINT ( 'NONE',  ( -30.29350689640809335, 120.5696653505793705, 16.00000000000000711 ) ) ;
#1927 = ORIENTED_EDGE ( 'NONE', *, *, #2415, .F. ) ;
#1928 = CARTESIAN_POINT ( 'NONE',  ( 0.000000000000000000, -133.1457019118818721, 27.15769640663938489 ) ) ;
#1929 = ORIENTED_EDGE ( 'NONE', *, *, #1491, .F. ) ;
#1930 =( NAMED_UNIT ( * ) SI_UNIT ( $, .STERADIAN. ) SOLID_ANGLE_UNIT ( ) );
#1931 = VERTEX_POINT ( 'NONE', #5291 ) ;
#1932 = EDGE_CURVE ( 'NONE', #7949, #5111, #3020, .T. ) ;
#1933 = AXIS2_PLACEMENT_3D ( 'NONE', #10415, #7768, #10210 ) ;
#1934 = DIRECTION ( 'NONE',  ( 1.000000000000000000, 0.000000000000000000, 0.000000000000000000 ) ) ;
#1935 = CARTESIAN_POINT ( 'NONE',  ( -16.29350689640809691, -8.660287962196477451, -5.025000000000002132 ) ) ;
#1936 = DIRECTION ( 'NONE',  ( -0.000000000000000000, 0.000000000000000000, -1.000000000000000000 ) ) ;
#1937 = DIRECTION ( 'NONE',  ( 0.000000000000000000, 0.000000000000000000, 1.000000000000000000 ) ) ;
#1938 = ORIENTED_EDGE ( 'NONE', *, *, #1440, .F. ) ;
#1939 = DIRECTION ( 'NONE',  ( 0.000000000000000000, 0.000000000000000000, 1.000000000000000000 ) ) ;
#1940 = ORIENTED_EDGE ( 'NONE', *, *, #6325, .T. ) ;
#1941 = AXIS2_PLACEMENT_3D ( 'NONE', #3340, #7420, #8211 ) ;
#1942 = PLANE ( 'NONE',  #7568 ) ;
#1943 = ORIENTED_EDGE ( 'NONE', *, *, #9980, .T. ) ;
#1944 = CARTESIAN_POINT ( 'NONE',  ( -27.15769640663940976, -133.1457019118818721, 27.15769640663938489 ) ) ;
#1945 = FACE_BOUND ( 'NONE', #479, .T. ) ;
#1946 = ORIENTED_EDGE ( 'NONE', *, *, #10327, .F. ) ;
#1947 = CARTESIAN_POINT ( 'NONE',  ( 53.40242741783141156, 52.77167129626698028, -30.00000000000000355 ) ) ;
#1948 = DIRECTION ( 'NONE',  ( 1.000000000000000000, -0.000000000000000000, -0.000000000000000000 ) ) ;
#1949 = EDGE_CURVE ( 'NONE', #1386, #1994, #5353, .T. ) ;
#1950 = DIRECTION ( 'NONE',  ( 1.000000000000000000, 6.106226635438360972E-16, 0.000000000000000000 ) ) ;
#1951 = DIRECTION ( 'NONE',  ( -0.7431448254773957984, 0.6691306063588565722, -0.000000000000000000 ) ) ;
#1952 = ORIENTED_EDGE ( 'NONE', *, *, #6956, .T. ) ;
#1953 = ORIENTED_EDGE ( 'NONE', *, *, #1068, .F. ) ;
#1954 = CIRCLE ( 'NONE', #8733, 3.999999999999989786 ) ;
#1955 = CARTESIAN_POINT ( 'NONE',  ( -2.293506896408097795, 147.5696653505793279, 30.00000000000000355 ) ) ;
#1956 =( NAMED_UNIT ( * ) PLANE_ANGLE_UNIT ( ) SI_UNIT ( $, .RADIAN. ) );
#1957 = AXIS2_PLACEMENT_3D ( 'NONE', #1834, #5062, #6496 ) ;
#1958 = FACE_OUTER_BOUND ( 'NONE', #8227, .T. ) ;
#1959 = EDGE_CURVE ( 'NONE', #8659, #9556, #6246, .T. ) ;
#1960 = LINE ( 'NONE', #5350, #1147 ) ;
#1961 = EDGE_CURVE ( 'NONE', #9616, #3561, #1325, .T. ) ;
#1962 = ORIENTED_EDGE ( 'NONE', *, *, #429, .T. ) ;
#1963 = DIRECTION ( 'NONE',  ( 0.000000000000000000, 1.000000000000000000, 0.000000000000000000 ) ) ;
#1964 = AXIS2_PLACEMENT_3D ( 'NONE', #5307, #5253, #4469 ) ;
#1965 = ORIENTED_EDGE ( 'NONE', *, *, #2549, .T. ) ;
#1966 = CIRCLE ( 'NONE', #5002, 3.000000000000000444 ) ;
#1967 = VERTEX_POINT ( 'NONE', #478 ) ;
#1968 = CARTESIAN_POINT ( 'NONE',  ( -25.15769640663940976, -117.1457019118819005, -1.756747170973246291E-14 ) ) ;
#1969 = DIRECTION ( 'NONE',  ( 1.000000000000000000, 0.000000000000000000, 0.000000000000000000 ) ) ;
#1970 = CIRCLE ( 'NONE', #4847, 7.500000000000000000 ) ;
#1971 = DIRECTION ( 'NONE',  ( -1.000000000000000000, 0.000000000000000000, 0.000000000000000000 ) ) ;
#1972 = CARTESIAN_POINT ( 'NONE',  ( -16.29350689640809691, -8.660287962196477451, -4.729641367753004033 ) ) ;
#1973 = EDGE_CURVE ( 'NONE', #9059, #5268, #7684, .T. ) ;
#1974 = EDGE_CURVE ( 'NONE', #6132, #623, #3668, .T. ) ;
#1975 = CIRCLE ( 'NONE', #8064, 3.999999999999999112 ) ;
#1976 = EDGE_CURVE ( 'NONE', #6245, #7785, #10233, .T. ) ;
#1977 = VECTOR ( 'NONE', #4423, 1000.000000000000000 ) ;
#1978 = CARTESIAN_POINT ( 'NONE',  ( -16.29350689640809691, -7.660287962196459688, 7.499999999999998224 ) ) ;
#1979 = EDGE_LOOP ( 'NONE', ( #4454, #3969, #492, #619 ) ) ;
#1980 = CARTESIAN_POINT ( 'NONE',  ( -126.4085176256957084, 224.6061440934676909, 0.000000000000000000 ) ) ;
#1981 = AXIS2_PLACEMENT_3D ( 'NONE', #1736, #2735, #4229 ) ;
#1982 = ORIENTED_EDGE ( 'NONE', *, *, #1581, .F. ) ;
#1983 = DIRECTION ( 'NONE',  ( 1.000000000000000000, -0.000000000000000000, -0.000000000000000000 ) ) ;
#1984 = CIRCLE ( 'NONE', #9268, 7.728925574020642841 ) ;
#1985 = EDGE_LOOP ( 'NONE', ( #9762, #3927 ) ) ;
#1986 = VECTOR ( 'NONE', #608, 1000.000000000000000 ) ;
#1987 = EDGE_CURVE ( 'NONE', #5429, #6933, #4007, .T. ) ;
#1988 = DIRECTION ( 'NONE',  ( 1.000000000000000000, 0.000000000000000000, 0.000000000000000000 ) ) ;
#1989 = CARTESIAN_POINT ( 'NONE',  ( -23.17384457509314544, 150.5696653505793563, 7.750000000000001776 ) ) ;
#1990 = FACE_OUTER_BOUND ( 'NONE', #9713, .T. ) ;
#1991 = CARTESIAN_POINT ( 'NONE',  ( 59.99999999999997868, -145.1457019118819005, 40.00000000000000000 ) ) ;
#1992 = ORIENTED_EDGE ( 'NONE', *, *, #2654, .T. ) ;
#1993 = CARTESIAN_POINT ( 'NONE',  ( -30.29350689640809335, 128.5696653505793847, 20.00000000000000711 ) ) ;
#1994 = VERTEX_POINT ( 'NONE', #10129 ) ;
#1995 = ADVANCED_FACE ( 'NONE', ( #9275 ), #5398, .F. ) ;
#1996 = ORIENTED_EDGE ( 'NONE', *, *, #5425, .T. ) ;
#1997 = CIRCLE ( 'NONE', #6046, 3.297986701801175258 ) ;
#1998 = LINE ( 'NONE', #7037, #7228 ) ;
#1999 = ORIENTED_EDGE ( 'NONE', *, *, #8846, .F. ) ;
#2000 = DIRECTION ( 'NONE',  ( 0.000000000000000000, 0.000000000000000000, -1.000000000000000000 ) ) ;
#2001 = CARTESIAN_POINT ( 'NONE',  ( -43.93820948810023452, 0.000000000000000000, 4.000000000000000000 ) ) ;
#2002 = FILL_AREA_STYLE_COLOUR ( '', #7784 ) ;
#2003 = DIRECTION ( 'NONE',  ( 1.000000000000000000, -0.000000000000000000, 0.000000000000000000 ) ) ;
#2004 = DIRECTION ( 'NONE',  ( -1.000000000000000000, 0.000000000000000000, 0.000000000000000000 ) ) ;
#2005 = AXIS2_PLACEMENT_3D ( 'NONE', #5768, #7427, #9118 ) ;
#2006 = DIRECTION ( 'NONE',  ( 0.000000000000000000, 0.000000000000000000, 1.000000000000000000 ) ) ;
#2007 = VERTEX_POINT ( 'NONE', #10178 ) ;
#2008 = ADVANCED_FACE ( 'NONE', ( #4603, #8474 ), #526, .F. ) ;
#2009 = ORIENTED_EDGE ( 'NONE', *, *, #3968, .F. ) ;
#2010 = CARTESIAN_POINT ( 'NONE',  ( -23.39899473324887680, -133.3869996355172987, -50.00000000000001421 ) ) ;
#2011 = ORIENTED_EDGE ( 'NONE', *, *, #6309, .F. ) ;
#2012 = CARTESIAN_POINT ( 'NONE',  ( 39.99999999999998579, -135.1457019118818721, -44.02500000000001990 ) ) ;
#2013 = CARTESIAN_POINT ( 'NONE',  ( -23.79350689640809691, 120.5289575273812233, 7.750000000000007105 ) ) ;
#2014 = VECTOR ( 'NONE', #4092, 1000.000000000000000 ) ;
#2015 = DIRECTION ( 'NONE',  ( 0.000000000000000000, -1.000000000000000000, 0.000000000000000000 ) ) ;
#2016 = CARTESIAN_POINT ( 'NONE',  ( 17.97972049165455388, 37.08684478514406635, -12.49999999999997335 ) ) ;
#2017 = VERTEX_POINT ( 'NONE', #6088 ) ;
#2018 = ADVANCED_BREP_SHAPE_REPRESENTATION ( '', ( #3318, #4601 ), #9900 ) ;
#2019 = VERTEX_POINT ( 'NONE', #2910 ) ;
#2020 = CARTESIAN_POINT ( 'NONE',  ( -48.00000000000002132, -115.1457019118818863, -23.15769640663945594 ) ) ;
#2021 = AXIS2_PLACEMENT_3D ( 'NONE', #6080, #8363, #4283 ) ;
#2022 = ADVANCED_FACE ( 'NONE', ( #9329 ), #10288, .F. ) ;
#2023 = ORIENTED_EDGE ( 'NONE', *, *, #6467, .F. ) ;
#2024 = DIRECTION ( 'NONE',  ( 0.000000000000000000, -1.000000000000000000, 0.000000000000000000 ) ) ;
#2025 = CARTESIAN_POINT ( 'NONE',  ( -2.293506896408097795, 42.08684478514406635, -25.00000000000000355 ) ) ;
#2026 = DIRECTION ( 'NONE',  ( 0.000000000000000000, 1.000000000000000000, 1.460512169908342690E-16 ) ) ;
#2027 = DIRECTION ( 'NONE',  ( -1.000000000000000000, 0.000000000000000000, 0.000000000000000000 ) ) ;
#2028 = CARTESIAN_POINT ( 'NONE',  ( 39.99999999999997158, -135.1457019118818721, 39.99999999999997868 ) ) ;
#2029 = ORIENTED_EDGE ( 'NONE', *, *, #5146, .F. ) ;
#2030 = DIRECTION ( 'NONE',  ( 0.000000000000000000, 0.000000000000000000, -1.000000000000000000 ) ) ;
#2031 = EDGE_CURVE ( 'NONE', #5603, #4869, #3842, .T. ) ;
#2032 = EDGE_CURVE ( 'NONE', #7226, #9088, #2221, .T. ) ;
#2033 = EDGE_CURVE ( 'NONE', #1605, #6079, #626, .T. ) ;
#2034 = CARTESIAN_POINT ( 'NONE',  ( -134.8713710537857935, 257.7072748320279061, 1.365612337163390183E-15 ) ) ;
#2035 = CARTESIAN_POINT ( 'NONE',  ( -30.29350689640809335, -0.3998014571812398832, 1.076388538564875708 ) ) ;
#2036 = FACE_BOUND ( 'NONE', #4461, .T. ) ;
#2037 = CARTESIAN_POINT ( 'NONE',  ( 37.23007123371004923, -133.6742494827832388, 25.22421275991299083 ) ) ;
#2038 = FACE_OUTER_BOUND ( 'NONE', #9675, .T. ) ;
#2039 = CARTESIAN_POINT ( 'NONE',  ( -163.4029438717996641, 273.7745032373030654, 4.898587196589562712E-16 ) ) ;
#2040 = ORIENTED_EDGE ( 'NONE', *, *, #441, .F. ) ;
#2041 = CIRCLE ( 'NONE', #6279, 7.785108809001807906 ) ;
#2042 = DIRECTION ( 'NONE',  ( 1.000000000000000000, 0.000000000000000000, 0.000000000000000000 ) ) ;
#2043 = ORIENTED_EDGE ( 'NONE', *, *, #1322, .T. ) ;
#2044 = ORIENTED_EDGE ( 'NONE', *, *, #10135, .T. ) ;
#2045 = ADVANCED_FACE ( 'NONE', ( #2966 ), #6194, .T. ) ;
#2046 = DIRECTION ( 'NONE',  ( 0.000000000000000000, -1.000000000000000000, 0.000000000000000000 ) ) ;
#2047 = ORIENTED_EDGE ( 'NONE', *, *, #9769, .F. ) ;
#2048 = AXIS2_PLACEMENT_3D ( 'NONE', #1868, #184, #916 ) ;
#2049 = ORIENTED_EDGE ( 'NONE', *, *, #3138, .F. ) ;
#2050 = CARTESIAN_POINT ( 'NONE',  ( 17.97972049165455388, 42.08684478514406635, -25.00000000000000000 ) ) ;
#2051 = DIRECTION ( 'NONE',  ( 0.000000000000000000, 0.000000000000000000, 1.000000000000000000 ) ) ;
#2052 = FACE_OUTER_BOUND ( 'NONE', #3019, .T. ) ;
#2053 = DIRECTION ( 'NONE',  ( -0.000000000000000000, 1.000000000000000000, -0.000000000000000000 ) ) ;
#2054 = CARTESIAN_POINT ( 'NONE',  ( -2.293506896408097795, 152.5696653505793279, -24.99999999999998934 ) ) ;
#2055 = CIRCLE ( 'NONE', #9857, 7.999999999999991118 ) ;
#2056 = EDGE_LOOP ( 'NONE', ( #10376, #7932, #1952 ) ) ;
#2057 = AXIS2_PLACEMENT_3D ( 'NONE', #8439, #3780, #342 ) ;
#2058 = ORIENTED_EDGE ( 'NONE', *, *, #1831, .F. ) ;
#2059 = CARTESIAN_POINT ( 'NONE',  ( -39.65624476065124782, -3.117691453623975484, -1.800000000000017586 ) ) ;
#2060 = ORIENTED_EDGE ( 'NONE', *, *, #9362, .T. ) ;
#2061 = CARTESIAN_POINT ( 'NONE',  ( -30.29350689640809335, 140.5696653505793563, -20.00000000000000355 ) ) ;
#2062 = LINE ( 'NONE', #4456, #8497 ) ;
#2063 = AXIS2_PLACEMENT_3D ( 'NONE', #186, #4990, #5102 ) ;
#2064 = VECTOR ( 'NONE', #8535, 1000.000000000000000 ) ;
#2065 = FACE_OUTER_BOUND ( 'NONE', #5158, .T. ) ;
#2066 = ADVANCED_FACE ( 'NONE', ( #8838, #3273 ), #1484, .T. ) ;
#2067 = CARTESIAN_POINT ( 'NONE',  ( -30.29350689640809335, 120.5696653505793705, 20.00000000000000711 ) ) ;
#2068 = ORIENTED_EDGE ( 'NONE', *, *, #3670, .F. ) ;
#2069 = VERTEX_POINT ( 'NONE', #6450 ) ;
#2070 = AXIS2_PLACEMENT_3D ( 'NONE', #10310, #6418, #10356 ) ;
#2071 = AXIS2_PLACEMENT_3D ( 'NONE', #831, #9802, #880 ) ;
#2072 = ORIENTED_EDGE ( 'NONE', *, *, #6556, .F. ) ;
#2073 = ORIENTED_EDGE ( 'NONE', *, *, #2722, .T. ) ;
#2074 = ORIENTED_EDGE ( 'NONE', *, *, #5847, .F. ) ;
#2075 = DIRECTION ( 'NONE',  ( -0.7431448254773956874, 0.6691306063588564612, -0.000000000000000000 ) ) ;
#2076 = SPHERICAL_SURFACE ( 'NONE', #2568, 2.000000000000000000 ) ;
#2077 = LINE ( 'NONE', #8491, #5687 ) ;
#2078 = DIRECTION ( 'NONE',  ( -0.000000000000000000, -1.000000000000000000, -0.000000000000000000 ) ) ;
#2079 = AXIS2_PLACEMENT_3D ( 'NONE', #2227, #7159, #8636 ) ;
#2080 = ADVANCED_FACE ( 'NONE', ( #4069 ), #6880, .T. ) ;
#2081 = DIRECTION ( 'NONE',  ( 0.000000000000000000, -1.000000000000000000, 0.000000000000000000 ) ) ;
#2082 = VERTEX_POINT ( 'NONE', #7302 ) ;
#2083 = CARTESIAN_POINT ( 'NONE',  ( -47.94539818030330025, 150.5696653505793563, -4.025000000000000355 ) ) ;
#2084 = CIRCLE ( 'NONE', #7345, 2.515249034521771510 ) ;
#2085 = ORIENTED_EDGE ( 'NONE', *, *, #8968, .F. ) ;
#2086 = CARTESIAN_POINT ( 'NONE',  ( -23.17384457509314899, 130.5696653505793847, 10.90000000000000036 ) ) ;
#2087 = PLANE ( 'NONE',  #9042 ) ;
#2088 = EDGE_CURVE ( 'NONE', #10220, #2586, #9750, .T. ) ;
#2089 = PLANE ( 'NONE',  #6695 ) ;
#2090 = CIRCLE ( 'NONE', #6156, 5.000000000000000000 ) ;
#2091 = EDGE_CURVE ( 'NONE', #4437, #10082, #8793, .T. ) ;
#2092 = ORIENTED_EDGE ( 'NONE', *, *, #8505, .T. ) ;
#2093 = DIRECTION ( 'NONE',  ( -1.000000000000000000, -0.000000000000000000, -0.000000000000000000 ) ) ;
#2094 = AXIS2_PLACEMENT_3D ( 'NONE', #6071, #258, #6713 ) ;
#2095 = EDGE_LOOP ( 'NONE', ( #1134, #4062, #1388, #6491, #7589 ) ) ;
#2096 = SHAPE_REPRESENTATION_RELATIONSHIP ( 'NONE' , 'NONE' ,  #5068, #6825 ) ;
#2097 = ORIENTED_EDGE ( 'NONE', *, *, #3900, .F. ) ;
#2098 = CARTESIAN_POINT ( 'NONE',  ( 77.30044127146538813, 73.68369600860394542, 25.00000000000000000 ) ) ;
#2099 =( BOUNDED_CURVE ( )  B_SPLINE_CURVE ( 3, ( #1856, #5086, #1059, #4291 ),
 .UNSPECIFIED., .F., .F. ) 
 B_SPLINE_CURVE_WITH_KNOTS ( ( 4, 4 ),
 ( 5.245636577995398397, 5.314071712302153472 ),
 .UNSPECIFIED. ) 
 CURVE ( )  GEOMETRIC_REPRESENTATION_ITEM ( )  RATIONAL_B_SPLINE_CURVE ( ( 1.000000000000000000, 0.9996097574442918132, 0.9996097574442918132, 1.000000000000000000 ) ) 
 REPRESENTATION_ITEM ( '' )  );
#2100 = ORIENTED_EDGE ( 'NONE', *, *, #3024, .F. ) ;
#2101 = AXIS2_PLACEMENT_3D ( 'NONE', #5351, #1132, #9189 ) ;
#2102 = VERTEX_POINT ( 'NONE', #1630 ) ;
#2103 = DIRECTION ( 'NONE',  ( 0.000000000000000000, 0.000000000000000000, 1.000000000000000000 ) ) ;
#2104 = DIRECTION ( 'NONE',  ( -1.000000000000000000, 0.000000000000000000, -0.000000000000000000 ) ) ;
#2105 = ORIENTED_EDGE ( 'NONE', *, *, #8613, .T. ) ;
#2106 = CARTESIAN_POINT ( 'NONE',  ( -16.29350689640809691, -140.1746510883711778, -7.500000000000000000 ) ) ;
#2107 = LINE ( 'NONE', #10065, #4468 ) ;
#2108 = EDGE_CURVE ( 'NONE', #4793, #8917, #10105, .T. ) ;
#2109 = ADVANCED_FACE ( 'NONE', ( #4712 ), #8093, .T. ) ;
#2110 = DIRECTION ( 'NONE',  ( -1.000000000000000000, 0.000000000000000000, 9.101836848464096770E-17 ) ) ;
#2111 = EDGE_CURVE ( 'NONE', #6094, #1253, #8920, .T. ) ;
#2112 = FACE_BOUND ( 'NONE', #4060, .T. ) ;
#2113 = TOROIDAL_SURFACE ( 'NONE', #6350, 4.000000000000000000, 2.000000000000000000 ) ;
#2114 = ORIENTED_EDGE ( 'NONE', *, *, #6996, .F. ) ;
#2115 = DIRECTION ( 'NONE',  ( -1.000000000000000000, 0.000000000000000000, 0.000000000000000000 ) ) ;
#2116 = AXIS2_PLACEMENT_3D ( 'NONE', #8691, #10346, #3824 ) ;
#2117 = EDGE_LOOP ( 'NONE', ( #4126, #8092, #5054, #10088 ) ) ;
#2118 = CARTESIAN_POINT ( 'NONE',  ( 6.250000000000005329, 0.000000000000000000, 3.000000000000000444 ) ) ;
#2119 = DIRECTION ( 'NONE',  ( 0.000000000000000000, 0.000000000000000000, -1.000000000000000000 ) ) ;
#2120 = CARTESIAN_POINT ( 'NONE',  ( 27.15769640663936713, -115.1457019118818863, 23.15769640663938134 ) ) ;
#2121 = EDGE_CURVE ( 'NONE', #6484, #6663, #2373, .T. ) ;
#2122 = ORIENTED_EDGE ( 'NONE', *, *, #10086, .F. ) ;
#2123 = ORIENTED_EDGE ( 'NONE', *, *, #5788, .F. ) ;
#2124 = PRODUCT_DEFINITION_SHAPE ( 'NONE', 'NONE',  #3203 ) ;
#2125 = EDGE_CURVE ( 'NONE', #9816, #288, #793, .T. ) ;
#2126 = VECTOR ( 'NONE', #3478, 1000.000000000000000 ) ;
#2127 = ORIENTED_EDGE ( 'NONE', *, *, #5471, .T. ) ;
#2128 = ORIENTED_EDGE ( 'NONE', *, *, #7497, .T. ) ;
#2129 = CARTESIAN_POINT ( 'NONE',  ( -16.29350689640809691, -115.1457019118818863, 27.01918567566963247 ) ) ;
#2130 = CARTESIAN_POINT ( 'NONE',  ( -16.29350689640809691, -8.660287962196477451, -6.499999999999964473 ) ) ;
#2131 = DIRECTION ( 'NONE',  ( -0.6585271261848815172, 0.7525569905852190766, -4.569449861441823711E-16 ) ) ;
#2132 = LINE ( 'NONE', #8492, #9187 ) ;
#2133 = VECTOR ( 'NONE', #3807, 1000.000000000000114 ) ;
#2134 = CARTESIAN_POINT ( 'NONE',  ( -40.00000000000002842, -145.1457019118819005, 49.99999999999997868 ) ) ;
#2135 = CIRCLE ( 'NONE', #8753, 7.862171649053781408 ) ;
#2136 = VERTEX_POINT ( 'NONE', #10338 ) ;
#2137 = LINE ( 'NONE', #6271, #5610 ) ;
#2138 = AXIS2_PLACEMENT_3D ( 'NONE', #427, #6890, #5241 ) ;
#2139 = DIRECTION ( 'NONE',  ( 1.000000000000000000, 0.000000000000000000, 8.379529552680124346E-16 ) ) ;
#2140 = ORIENTED_EDGE ( 'NONE', *, *, #9977, .T. ) ;
#2141 = VECTOR ( 'NONE', #10230, 1000.000000000000000 ) ;
#2142 = DIRECTION ( 'NONE',  ( 0.000000000000000000, 0.000000000000000000, -1.000000000000000000 ) ) ;
#2143 = CARTESIAN_POINT ( 'NONE',  ( -56.34457570605425758, 137.0132282531173473, 3.999999999999976019 ) ) ;
#2144 = CARTESIAN_POINT ( 'NONE',  ( -50.00000000000002132, -115.1457019118818863, -6.938893903907231533E-15 ) ) ;
#2145 = CIRCLE ( 'NONE', #2819, 4.000000000000000000 ) ;
#2146 = VERTEX_POINT ( 'NONE', #3066 ) ;
#2147 = DIRECTION ( 'NONE',  ( 1.396588258780021135E-16, 0.000000000000000000, 1.000000000000000000 ) ) ;
#2148 = VECTOR ( 'NONE', #4795, 1000.000000000000000 ) ;
#2149 = ORIENTED_EDGE ( 'NONE', *, *, #7672, .F. ) ;
#2150 = APPLICATION_PROTOCOL_DEFINITION ( 'draft international standard', 'automotive_design', 1998, #6258 ) ;
#2151 = ORIENTED_EDGE ( 'NONE', *, *, #4357, .T. ) ;
#2152 = CYLINDRICAL_SURFACE ( 'NONE', #6213, 4.729641367753004033 ) ;
#2153 = EDGE_CURVE ( 'NONE', #2439, #2342, #3160, .T. ) ;
#2154 = VERTEX_POINT ( 'NONE', #8739 ) ;
#2155 = AXIS2_PLACEMENT_3D ( 'NONE', #7971, #21, #3044 ) ;
#2156 = ORIENTED_EDGE ( 'NONE', *, *, #5857, .T. ) ;
#2157 = CYLINDRICAL_SURFACE ( 'NONE', #3488, 5.000000000000000888 ) ;
#2158 = LINE ( 'NONE', #8124, #1049 ) ;
#2159 = ORIENTED_EDGE ( 'NONE', *, *, #9094, .F. ) ;
#2161 = EDGE_CURVE ( 'NONE', #3561, #6261, #3170, .T. ) ;
#2160 = CARTESIAN_POINT ( 'NONE',  ( 14.70649310359190309, 80.56966535057935630, -20.00000000000000711 ) ) ;
#2162 = AXIS2_PLACEMENT_3D ( 'NONE', #9579, #10209, #2142 ) ;
#2163 = DIRECTION ( 'NONE',  ( -0.6691306063588601249, -0.7431448254773928008, 0.000000000000000000 ) ) ;
#2164 = DIRECTION ( 'NONE',  ( 0.000000000000000000, 0.000000000000000000, -1.000000000000000000 ) ) ;
#2165 = DIRECTION ( 'NONE',  ( -0.000000000000000000, 1.000000000000000000, 0.000000000000000000 ) ) ;
#2166 = DIRECTION ( 'NONE',  ( 1.000000000000000000, -0.000000000000000000, -0.000000000000000000 ) ) ;
#2167 = VECTOR ( 'NONE', #9926, 1000.000000000000000 ) ;
#2168 = EDGE_LOOP ( 'NONE', ( #6812, #9545, #7693, #8510 ) ) ;
#2169 = CARTESIAN_POINT ( 'NONE',  ( 23.15769640663940265, -115.1457019118818863, -48.00000000000002132 ) ) ;
#2170 = EDGE_CURVE ( 'NONE', #5671, #2596, #7914, .T. ) ;
#2171 = EDGE_CURVE ( 'NONE', #8901, #3840, #9435, .T. ) ;
#2172 = EDGE_CURVE ( 'NONE', #10246, #382, #5558, .T. ) ;
#2173 = ORIENTED_EDGE ( 'NONE', *, *, #8842, .T. ) ;
#2174 = DIRECTION ( 'NONE',  ( 0.000000000000000000, 0.000000000000000000, 1.000000000000000000 ) ) ;
#2175 = CARTESIAN_POINT ( 'NONE',  ( 27.15769640663936713, -117.1457019118819005, 27.15769640663938489 ) ) ;
#2176 = AXIS2_PLACEMENT_3D ( 'NONE', #2955, #1586, #8257 ) ;
#2177 = SPHERICAL_SURFACE ( 'NONE', #3783, 2.000000000000000000 ) ;
#2178 = CARTESIAN_POINT ( 'NONE',  ( -2.293506896408097795, 152.5696653505793279, -30.00000000000000355 ) ) ;
#2179 = CARTESIAN_POINT ( 'NONE',  ( 38.19229777560031636, -43.28483205141633761, -12.50000000000000000 ) ) ;
#2180 = AXIS2_PLACEMENT_3D ( 'NONE', #5276, #767, #7880 ) ;
#2181 = ORIENTED_EDGE ( 'NONE', *, *, #3367, .F. ) ;
#2182 = VERTEX_POINT ( 'NONE', #4752 ) ;
#2183 = ORIENTED_EDGE ( 'NONE', *, *, #744, .F. ) ;
#2184 = EDGE_CURVE ( 'NONE', #7051, #7422, #1580, .T. ) ;
#2185 = VECTOR ( 'NONE', #4044, 1000.000000000000000 ) ;
#2186 = VERTEX_POINT ( 'NONE', #4804 ) ;
#2187 = CARTESIAN_POINT ( 'NONE',  ( -2.293506896408097795, 152.5696653505793279, 30.00000000000000355 ) ) ;
#2188 = DIRECTION ( 'NONE',  ( -8.194486552889013533E-17, -9.100899318238110877E-17, 1.000000000000000000 ) ) ;
#2189 = DIRECTION ( 'NONE',  ( 0.000000000000000000, 0.000000000000000000, 1.000000000000000000 ) ) ;
#2190 = LINE ( 'NONE', #6797, #8845 ) ;
#2191 = LINE ( 'NONE', #3038, #1469 ) ;
#2192 = VERTEX_POINT ( 'NONE', #8040 ) ;
#2193 = CIRCLE ( 'NONE', #3040, 4.000000000000000000 ) ;
#2194 = CARTESIAN_POINT ( 'NONE',  ( -121.7299640054770578, 230.8694527092982867, 0.000000000000000000 ) ) ;
#2195 = ORIENTED_EDGE ( 'NONE', *, *, #4051, .T. ) ;
#2196 = ORIENTED_EDGE ( 'NONE', *, *, #7267, .T. ) ;
#2197 = LINE ( 'NONE', #2831, #9091 ) ;
#2198 = CARTESIAN_POINT ( 'NONE',  ( -47.94539818030330025, 137.0132282531173473, -3.999999999999991562 ) ) ;
#2199 = DIRECTION ( 'NONE',  ( 0.000000000000000000, 0.000000000000000000, -1.000000000000000000 ) ) ;
#2200 = EDGE_CURVE ( 'NONE', #8048, #6849, #4023, .T. ) ;
#2201 = DIRECTION ( 'NONE',  ( -1.000000000000000000, 0.000000000000000000, 0.000000000000000000 ) ) ;
#2202 = EDGE_LOOP ( 'NONE', ( #7733, #10267, #3875, #7881, #9652 ) ) ;
#2203 = CARTESIAN_POINT ( 'NONE',  ( 17.97972049165455388, 42.08684478514406635, 30.00000000000000355 ) ) ;
#2204 = ORIENTED_EDGE ( 'NONE', *, *, #6543, .F. ) ;
#2205 = CARTESIAN_POINT ( 'NONE',  ( 0.000000000000000000, 0.000000000000000000, 0.000000000000000000 ) ) ;
#2206 = EDGE_LOOP ( 'NONE', ( #2312, #10473, #7213, #131 ) ) ;
#2207 = DIRECTION ( 'NONE',  ( 0.000000000000000000, -0.5000000000000011102, -0.8660254037844379305 ) ) ;
#2208 = ORIENTED_EDGE ( 'NONE', *, *, #4655, .F. ) ;
#2209 = VERTEX_POINT ( 'NONE', #5968 ) ;
#2210 = CARTESIAN_POINT ( 'NONE',  ( 3.000000000000000000, 1.467624384280032501, 2.541999999999999371 ) ) ;
#2211 = DIRECTION ( 'NONE',  ( 0.7431448254773962425, -0.6691306063588559061, 0.000000000000000000 ) ) ;
#2212 = VERTEX_POINT ( 'NONE', #8302 ) ;
#2213 = DIRECTION ( 'NONE',  ( -0.6761648913424331830, 0.7367503238654705688, 0.000000000000000000 ) ) ;
#2214 = CARTESIAN_POINT ( 'NONE',  ( -67.94539818030330025, 155.5289575273812090, 0.000000000000000000 ) ) ;
#2215 = FACE_OUTER_BOUND ( 'NONE', #4543, .T. ) ;
#2216 = CARTESIAN_POINT ( 'NONE',  ( -25.15769640663937423, -117.1457019118819005, -48.00000000000002132 ) ) ;
#2217 = CARTESIAN_POINT ( 'NONE',  ( 53.40242741783141156, 52.77167129626698028, 30.00000000000000355 ) ) ;
#2218 = PRODUCT_DEFINITION_SHAPE ( 'NONE', 'NONE',  #6773 ) ;
#2219 = EDGE_CURVE ( 'NONE', #288, #9816, #5526, .T. ) ;
#2220 = ORIENTED_EDGE ( 'NONE', *, *, #1243, .T. ) ;
#2221 = LINE ( 'NONE', #6140, #3154 ) ;
#2222 = AXIS2_PLACEMENT_3D ( 'NONE', #6885, #2165, #9218 ) ;
#2223 = EDGE_LOOP ( 'NONE', ( #3669, #9856, #2555, #8359 ) ) ;
#2224 = DIRECTION ( 'NONE',  ( 0.000000000000000000, 0.000000000000000000, -1.000000000000000000 ) ) ;
#2225 = FACE_BOUND ( 'NONE', #4473, .T. ) ;
#2226 = ORIENTED_EDGE ( 'NONE', *, *, #1098, .F. ) ;
#2227 = CARTESIAN_POINT ( 'NONE',  ( -16.29350689640809691, -8.660287962196477451, 0.000000000000000000 ) ) ;
#2228 = DIRECTION ( 'NONE',  ( 0.000000000000000000, 0.000000000000000000, 1.000000000000000000 ) ) ;
#2229 = AXIS2_PLACEMENT_3D ( 'NONE', #5948, #10096, #2878 ) ;
#2230 = CARTESIAN_POINT ( 'NONE',  ( -20.29350689640809691, 140.5696653505793563, 20.00000000000002132 ) ) ;
#2231 = VECTOR ( 'NONE', #1195, 1000.000000000000000 ) ;
#2232 = ORIENTED_EDGE ( 'NONE', *, *, #6583, .T. ) ;
#2233 = EDGE_CURVE ( 'NONE', #5001, #8168, #7460, .T. ) ;
#2234 = ADVANCED_FACE ( 'NONE', ( #10010 ), #3329, .F. ) ;
#2235 = ADVANCED_FACE ( 'NONE', ( #5810 ), #7567, .F. ) ;
#2236 = EDGE_LOOP ( 'NONE', ( #1376, #7614, #1473, #10387 ) ) ;
#2237 = VECTOR ( 'NONE', #3122, 1000.000000000000000 ) ;
#2238 = EDGE_LOOP ( 'NONE', ( #3655, #6176 ) ) ;
#2239 = ORIENTED_EDGE ( 'NONE', *, *, #5458, .F. ) ;
#2240 = CARTESIAN_POINT ( 'NONE',  ( -16.29350689640809691, -186.9457019118818835, 27.01918567566963247 ) ) ;
#2241 = LINE ( 'NONE', #8648, #9006 ) ;
#2242 = FACE_OUTER_BOUND ( 'NONE', #417, .T. ) ;
#2243 = DIRECTION ( 'NONE',  ( 0.000000000000000000, 0.000000000000000000, 1.000000000000000000 ) ) ;
#2244 = FACE_OUTER_BOUND ( 'NONE', #5322, .T. ) ;
#2245 = EDGE_CURVE ( 'NONE', #1079, #7959, #5067, .T. ) ;
#2246 = AXIS2_PLACEMENT_3D ( 'NONE', #5492, #10275, #7334 ) ;
#2247 = EDGE_CURVE ( 'NONE', #10447, #4228, #7356, .T. ) ;
#2248 = ORIENTED_EDGE ( 'NONE', *, *, #7081, .T. ) ;
#2249 = VECTOR ( 'NONE', #2042, 1000.000000000000000 ) ;
#2250 = CARTESIAN_POINT ( 'NONE',  ( -111.3540224549888933, 212.1074838665961124, 0.000000000000000000 ) ) ;
#2251 = ORIENTED_EDGE ( 'NONE', *, *, #3281, .T. ) ;
#2252 = DIRECTION ( 'NONE',  ( -0.7431448254773957984, 0.6691306063588565722, -0.000000000000000000 ) ) ;
#2253 = VECTOR ( 'NONE', #8388, 1000.000000000000000 ) ;
#2254 = CARTESIAN_POINT ( 'NONE',  ( 77.30044127146538813, 73.68369600860394542, 30.00000000000000355 ) ) ;
#2255 = LINE ( 'NONE', #5375, #5826 ) ;
#2256 = DIRECTION ( 'NONE',  ( -1.000000000000000000, -0.000000000000000000, -0.000000000000000000 ) ) ;
#2257 = ORIENTED_EDGE ( 'NONE', *, *, #5471, .F. ) ;
#2258 = CARTESIAN_POINT ( 'NONE',  ( -3.173844575093148990, 130.5696653505793847, 7.750000000000000000 ) ) ;
#2259 = VECTOR ( 'NONE', #9983, 1000.000000000000000 ) ;
#2260 = CARTESIAN_POINT ( 'NONE',  ( -36.29350689640809691, 80.56966535057935630, -20.00000000000001066 ) ) ;
#2261 = VERTEX_POINT ( 'NONE', #1790 ) ;
#2262 = CARTESIAN_POINT ( 'NONE',  ( -7.293506896408097795, 80.56966535057935630, -20.00000000000000711 ) ) ;
#2263 = ORIENTED_EDGE ( 'NONE', *, *, #4916, .T. ) ;
#2264 = EDGE_CURVE ( 'NONE', #6316, #7078, #98, .T. ) ;
#2265 = APPLICATION_CONTEXT ( 'automotive_design' ) ;
#2266 = EDGE_LOOP ( 'NONE', ( #5185, #8963, #9468, #1255 ) ) ;
#2267 = DIRECTION ( 'NONE',  ( 0.1124875939035003825, 0.8966615917995841567, 0.4281874951574803356 ) ) ;
#2268 = LINE ( 'NONE', #9479, #5275 ) ;
#2269 = AXIS2_PLACEMENT_3D ( 'NONE', #6346, #1477, #1369 ) ;
#2270 = DIRECTION ( 'NONE',  ( -0.7367503238654704578, -0.6761648913424330720, 0.000000000000000000 ) ) ;
#2271 = CYLINDRICAL_SURFACE ( 'NONE', #1760, 4.000000000000016875 ) ;
#2272 = CARTESIAN_POINT ( 'NONE',  ( 23.15769640663936713, -135.1457019118818721, 47.99999999999997868 ) ) ;
#2273 = CARTESIAN_POINT ( 'NONE',  ( 23.15769640663936713, -117.1457019118819005, 47.99999999999997868 ) ) ;
#2274 = LINE ( 'NONE', #8789, #5355 ) ;
#2275 = VERTEX_POINT ( 'NONE', #5124 ) ;
#2276 = AXIS2_PLACEMENT_3D ( 'NONE', #5443, #4747, #3162 ) ;
#2277 = CARTESIAN_POINT ( 'NONE',  ( 6.000000000000005329, 5.000000000000000000, 0.000000000000000000 ) ) ;
#2278 =( GEOMETRIC_REPRESENTATION_CONTEXT ( 3 ) GLOBAL_UNCERTAINTY_ASSIGNED_CONTEXT ( ( #3360 ) ) GLOBAL_UNIT_ASSIGNED_CONTEXT ( ( #7398, #6601, #9089 ) ) REPRESENTATION_CONTEXT ( 'NONE', 'WORKASPACE' ) );
#2279 = ORIENTED_EDGE ( 'NONE', *, *, #1200, .F. ) ;
#2280 = EDGE_CURVE ( 'NONE', #47, #2630, #5172, .T. ) ;
#2281 = DIRECTION ( 'NONE',  ( -0.000000000000000000, 1.000000000000000000, 0.000000000000000000 ) ) ;
#2282 = LINE ( 'NONE', #5402, #1041 ) ;
#2283 = CARTESIAN_POINT ( 'NONE',  ( -20.29350689640809691, 140.5696653505793563, 10.90000000000000036 ) ) ;
#2284 = FACE_OUTER_BOUND ( 'NONE', #1032, .T. ) ;
#2285 = AXIS2_PLACEMENT_3D ( 'NONE', #5480, #1409, #7817 ) ;
#2286 = LINE ( 'NONE', #5661, #8210 ) ;
#2287 = ORIENTED_EDGE ( 'NONE', *, *, #7815, .F. ) ;
#2288 = VERTEX_POINT ( 'NONE', #5015 ) ;
#2289 = AXIS2_PLACEMENT_3D ( 'NONE', #4666, #5460, #10393 ) ;
#2290 = ORIENTED_EDGE ( 'NONE', *, *, #302, .F. ) ;
#2291 = ORIENTED_EDGE ( 'NONE', *, *, #9502, .F. ) ;
#2292 = ADVANCED_FACE ( 'NONE', ( #5913 ), #1942, .T. ) ;
#2293 = FACE_BOUND ( 'NONE', #2238, .T. ) ;
#2294 = CARTESIAN_POINT ( 'NONE',  ( 23.64290342185648797, -133.6308916829187297, 49.99999999999999289 ) ) ;
#2295 = DIRECTION ( 'NONE',  ( 6.982941293900105430E-16, 0.000000000000000000, -1.000000000000000000 ) ) ;
#2296 = DIRECTION ( 'NONE',  ( -0.6691306063588566833, -0.7431448254773956874, 0.000000000000000000 ) ) ;
#2297 = DIRECTION ( 'NONE',  ( -0.000000000000000000, 0.000000000000000000, 1.000000000000000000 ) ) ;
#2298 = ORIENTED_EDGE ( 'NONE', *, *, #5367, .T. ) ;
#2299 = LINE ( 'NONE', #503, #7810 ) ;
#2300 = CIRCLE ( 'NONE', #1460, 4.729641367753004033 ) ;
#2301 = ORIENTED_EDGE ( 'NONE', *, *, #3837, .F. ) ;
#2302 = ADVANCED_FACE ( 'NONE', ( #9968 ), #6560, .T. ) ;
#2303 = CYLINDRICAL_SURFACE ( 'NONE', #965, 2.000000000000001776 ) ;
#2304 = EDGE_CURVE ( 'NONE', #9783, #4360, #4173, .T. ) ;
#2305 = AXIS2_PLACEMENT_3D ( 'NONE', #2560, #8387, #4365 ) ;
#2306 = EDGE_CURVE ( 'NONE', #4058, #5577, #2145, .T. ) ;
#2307 = PRODUCT ( 'Primary Joint', 'Primary Joint', '', ( #2315 ) ) ;
#2308 = VECTOR ( 'NONE', #4326, 1000.000000000000114 ) ;
#2309 = DIRECTION ( 'NONE',  ( -0.000000000000000000, -0.000000000000000000, -1.000000000000000000 ) ) ;
#2310 = DIRECTION ( 'NONE',  ( -0.7525569905852205199, -0.6585271261848794078, 0.000000000000000000 ) ) ;
#2311 = CARTESIAN_POINT ( 'NONE',  ( 42.22511195853866184, 52.77167129626698028, 25.00000000000000000 ) ) ;
#2312 = ORIENTED_EDGE ( 'NONE', *, *, #317, .F. ) ;
#2313 = LINE ( 'NONE', #2203, #4609 ) ;
#2314 = VECTOR ( 'NONE', #7963, 1000.000000000000000 ) ;
#2315 = PRODUCT_CONTEXT ( 'NONE', #646, 'mechanical' ) ;
#2316 = ORIENTED_EDGE ( 'NONE', *, *, #5596, .T. ) ;
#2317 = AXIS2_PLACEMENT_3D ( 'NONE', #6483, #922, #7389 ) ;
#2318 = DIRECTION ( 'NONE',  ( -1.000000000000000000, 0.000000000000000000, 0.000000000000000000 ) ) ;
#2319 = ORIENTED_EDGE ( 'NONE', *, *, #905, .F. ) ;
#2320 = ADVANCED_FACE ( 'NONE', ( #6609 ), #8357, .T. ) ;
#2321 = PLANE ( 'NONE',  #10432 ) ;
#2322 = VECTOR ( 'NONE', #5327, 1000.000000000000000 ) ;
#2323 = DIRECTION ( 'NONE',  ( 0.000000000000000000, 0.000000000000000000, 1.000000000000000000 ) ) ;
#2324 = CARTESIAN_POINT ( 'NONE',  ( 27.15769640663936713, -117.1457019118819005, 25.15769640663938134 ) ) ;
#2325 = AXIS2_PLACEMENT_3D ( 'NONE', #9623, #9776, #5624 ) ;
#2326 = DIRECTION ( 'NONE',  ( 0.000000000000000000, 1.000000000000000000, -0.000000000000000000 ) ) ;
#2327 = COLOUR_RGB ( '',0.7921568627450980005, 0.8196078431372548767, 0.9333333333333333481 ) ;
#2328 = CARTESIAN_POINT ( 'NONE',  ( -50.00000000000001421, -135.1457019118818721, -40.00000000000002132 ) ) ;
#2329 = ORIENTED_EDGE ( 'NONE', *, *, #9097, .F. ) ;
#2330 = DIRECTION ( 'NONE',  ( 1.000000000000000000, 0.000000000000000000, 0.000000000000000000 ) ) ;
#2331 = AXIS2_PLACEMENT_3D ( 'NONE', #7792, #7588, #7005 ) ;
#2332 = ORIENTED_EDGE ( 'NONE', *, *, #7411, .T. ) ;
#2333 = DIRECTION ( 'NONE',  ( 1.000000000000000000, 0.000000000000000000, 1.387778780781445676E-16 ) ) ;
#2334 = SURFACE_STYLE_USAGE ( .BOTH. , #6404 ) ;
#2335 = DIRECTION ( 'NONE',  ( 1.000000000000000000, 0.000000000000000000, 0.000000000000000000 ) ) ;
#2336 = VECTOR ( 'NONE', #3062, 1000.000000000000000 ) ;
#2337 = VECTOR ( 'NONE', #10307, 1000.000000000000000 ) ;
#2338 = DIRECTION ( 'NONE',  ( -1.000000000000000000, -0.000000000000000000, -0.000000000000000000 ) ) ;
#2339 = VERTEX_POINT ( 'NONE', #1097 ) ;
#2340 = EDGE_CURVE ( 'NONE', #10187, #1889, #5692, .T. ) ;
#2341 = ORIENTED_EDGE ( 'NONE', *, *, #5916, .T. ) ;
#2342 = VERTEX_POINT ( 'NONE', #1839 ) ;
#2343 = FACE_BOUND ( 'NONE', #1146, .T. ) ;
#2344 = CARTESIAN_POINT ( 'NONE',  ( 27.15769640663936713, -133.1457019118818721, 25.15769640663938134 ) ) ;
#2345 = VECTOR ( 'NONE', #5435, 1000.000000000000000 ) ;
#2346 = CARTESIAN_POINT ( 'NONE',  ( -133.6038276124207300, 241.5607275224312787, 0.000000000000000000 ) ) ;
#2347 = FACE_OUTER_BOUND ( 'NONE', #9830, .T. ) ;
#2348 = AXIS2_PLACEMENT_3D ( 'NONE', #6563, #3221, #8145 ) ;
#2349 = ORIENTED_EDGE ( 'NONE', *, *, #2669, .T. ) ;
#2350 = FACE_OUTER_BOUND ( 'NONE', #6872, .T. ) ;
#2351 = ADVANCED_FACE ( 'NONE', ( #3543 ), #1136, .T. ) ;
#2352 = VECTOR ( 'NONE', #6005, 1000.000000000000000 ) ;
#2353 = ORIENTED_EDGE ( 'NONE', *, *, #8199, .T. ) ;
#2354 = DIRECTION ( 'NONE',  ( 0.000000000000000000, 0.000000000000000000, -1.000000000000000000 ) ) ;
#2355 = CARTESIAN_POINT ( 'NONE',  ( 27.15769640663936713, -115.1457019118818863, 27.15769640663938489 ) ) ;
#2356 = CARTESIAN_POINT ( 'NONE',  ( -2.293506896408097795, 37.08684478514406635, 0.000000000000000000 ) ) ;
#2357 = VERTEX_POINT ( 'NONE', #4279 ) ;
#2358 = DIRECTION ( 'NONE',  ( 0.000000000000000000, 0.000000000000000000, 1.000000000000000000 ) ) ;
#2359 = ADVANCED_FACE ( 'NONE', ( #8619 ), #1475, .F. ) ;
#2360 = EDGE_CURVE ( 'NONE', #1028, #5001, #6233, .T. ) ;
#2361 = ADVANCED_FACE ( 'NONE', ( #9368 ), #10165, .T. ) ;
#2362 = VERTEX_POINT ( 'NONE', #2842 ) ;
#2363 = DIRECTION ( 'NONE',  ( 0.000000000000000000, 0.000000000000000000, -1.000000000000000000 ) ) ;
#2364 = CIRCLE ( 'NONE', #8286, 4.000000000000000000 ) ;
#2365 = ORIENTED_EDGE ( 'NONE', *, *, #5529, .F. ) ;
#2366 = CARTESIAN_POINT ( 'NONE',  ( -50.00000000000001421, -135.1457019118818721, -26.62179802177720944 ) ) ;
#2367 = DIRECTION ( 'NONE',  ( -0.000000000000000000, -1.000000000000000000, -0.000000000000000000 ) ) ;
#2368 = DIRECTION ( 'NONE',  ( 0.000000000000000000, 0.000000000000000000, -1.000000000000000000 ) ) ;
#2369 = DIRECTION ( 'NONE',  ( -0.000000000000000000, -0.000000000000000000, -1.000000000000000000 ) ) ;
#2370 = CARTESIAN_POINT ( 'NONE',  ( 80.08610854271792334, 54.73418909528891874, 25.00000000000000000 ) ) ;
#2371 = EDGE_CURVE ( 'NONE', #1314, #3326, #1970, .T. ) ;
#2372 = EDGE_LOOP ( 'NONE', ( #3117, #8725 ) ) ;
#2373 = LINE ( 'NONE', #9601, #5862 ) ;
#2374 = ORIENTED_EDGE ( 'NONE', *, *, #981, .T. ) ;
#2375 = DIRECTION ( 'NONE',  ( -1.137729606058012035E-16, -0.000000000000000000, -1.000000000000000000 ) ) ;
#2376 =( NAMED_UNIT ( * ) PLANE_ANGLE_UNIT ( ) SI_UNIT ( $, .RADIAN. ) );
#2377 = CARTESIAN_POINT ( 'NONE',  ( 0.000000000000000000, 2.935248768560057897, -3.252606517456513302E-15 ) ) ;
#2378 = LINE ( 'NONE', #8800, #577 ) ;
#2379 = DIRECTION ( 'NONE',  ( -0.7431448254773957984, 0.6691306063588565722, -0.000000000000000000 ) ) ;
#2380 = EDGE_LOOP ( 'NONE', ( #8279, #9, #5242, #2072 ) ) ;
#2381 = ORIENTED_EDGE ( 'NONE', *, *, #2399, .F. ) ;
#2382 = VECTOR ( 'NONE', #6443, 1000.000000000000000 ) ;
#2383 = ORIENTED_EDGE ( 'NONE', *, *, #1163, .F. ) ;
#2384 = DIRECTION ( 'NONE',  ( -0.000000000000000000, 1.000000000000000000, -0.000000000000000000 ) ) ;
#2385 = ADVANCED_FACE ( 'NONE', ( #2949 ), #2152, .F. ) ;
#2386 = CARTESIAN_POINT ( 'NONE',  ( 24.98775663295400307, -134.6884760388430777, 49.99999999999998579 ) ) ;
#2387 = ORIENTED_EDGE ( 'NONE', *, *, #6169, .F. ) ;
#2388 =( GEOMETRIC_REPRESENTATION_CONTEXT ( 3 ) GLOBAL_UNCERTAINTY_ASSIGNED_CONTEXT ( ( #9833 ) ) GLOBAL_UNIT_ASSIGNED_CONTEXT ( ( #1764, #4099, #4255 ) ) REPRESENTATION_CONTEXT ( 'NONE', 'WORKASPACE' ) );
#2389 = FACE_OUTER_BOUND ( 'NONE', #6953, .T. ) ;
#2390 = PLANE ( 'NONE',  #10373 ) ;
#2391 = VERTEX_POINT ( 'NONE', #2893 ) ;
#2392 = CARTESIAN_POINT ( 'NONE',  ( -47.94539818030328604, 155.5289575273811522, 0.000000000000000000 ) ) ;
#2393 = EDGE_LOOP ( 'NONE', ( #10409, #10009, #5914, #216 ) ) ;
#2394 = SURFACE_STYLE_USAGE ( .BOTH. , #1603 ) ;
#2395 = COLOUR_RGB ( '',0.7921568627450980005, 0.8196078431372548767, 0.9333333333333333481 ) ;
#2396 = CONICAL_SURFACE ( 'NONE', #713, 4.025000000000000355, 0.7853981633975870569 ) ;
#2397 = ORIENTED_EDGE ( 'NONE', *, *, #7618, .T. ) ;
#2398 = CARTESIAN_POINT ( 'NONE',  ( -7.293506896408097795, 0.000000000000000000, 0.000000000000000000 ) ) ;
#2399 = EDGE_CURVE ( 'NONE', #4328, #3441, #1998, .T. ) ;
#2400 = CIRCLE ( 'NONE', #10198, 3.999999999999989786 ) ;
#2401 = AXIS2_PLACEMENT_3D ( 'NONE', #669, #1358, #1465 ) ;
#2402 = DIRECTION ( 'NONE',  ( 0.000000000000000000, 0.000000000000000000, 1.000000000000000000 ) ) ;
#2403 = CARTESIAN_POINT ( 'NONE',  ( 37.31847924783638604, -134.7590046800779930, -25.96838025129187599 ) ) ;
#2404 = VERTEX_POINT ( 'NONE', #465 ) ;
#2405 = CARTESIAN_POINT ( 'NONE',  ( -16.29350689640809691, -186.9457019118818835, 30.31717237747080773 ) ) ;
#2406 = APPLICATION_PROTOCOL_DEFINITION ( 'draft international standard', 'automotive_design', 1998, #3352 ) ;
#2407 = EDGE_LOOP ( 'NONE', ( #8584, #3415 ) ) ;
#2408 = AXIS2_PLACEMENT_3D ( 'NONE', #1870, #344, #4153 ) ;
#2409 = DIRECTION ( 'NONE',  ( 1.000000000000000000, 0.000000000000000000, 0.000000000000000000 ) ) ;
#2410 = VECTOR ( 'NONE', #4214, 1000.000000000000000 ) ;
#2411 = AXIS2_PLACEMENT_3D ( 'NONE', #2217, #3216, #9650 ) ;
#2412 = ORIENTED_EDGE ( 'NONE', *, *, #2808, .T. ) ;
#2413 = ORIENTED_EDGE ( 'NONE', *, *, #7111, .F. ) ;
#2414 = EDGE_CURVE ( 'NONE', #9655, #4137, #10114, .T. ) ;
#2415 = EDGE_CURVE ( 'NONE', #2815, #4536, #6126, .T. ) ;
#2416 = FACE_BOUND ( 'NONE', #1291, .T. ) ;
#2417 = DIRECTION ( 'NONE',  ( 0.000000000000000000, 0.000000000000000000, 1.000000000000000000 ) ) ;
#2418 = CARTESIAN_POINT ( 'NONE',  ( 0.000000000000000000, -117.1457019118819005, 49.99999999999997868 ) ) ;
#2419 = AXIS2_PLACEMENT_3D ( 'NONE', #9172, #3353, #8112 ) ;
#2420 = DIRECTION ( 'NONE',  ( 0.000000000000000000, -1.000000000000000000, 0.000000000000000000 ) ) ;
#2421 = DIRECTION ( 'NONE',  ( 0.000000000000000000, 1.224646799147353207E-16, -1.000000000000000000 ) ) ;
#2422 = ORIENTED_EDGE ( 'NONE', *, *, #8582, .T. ) ;
#2423 = DIRECTION ( 'NONE',  ( 0.000000000000000000, 0.000000000000000000, -1.000000000000000000 ) ) ;
#2424 = VECTOR ( 'NONE', #2003, 1000.000000000000000 ) ;
#2425 = VERTEX_POINT ( 'NONE', #6929 ) ;
#2426 = LINE ( 'NONE', #8096, #2852 ) ;
#2427 = EDGE_CURVE ( 'NONE', #2261, #7537, #514, .T. ) ;
#2428 = CARTESIAN_POINT ( 'NONE',  ( -115.3226892516804583, 225.1003166080523954, 0.000000000000000000 ) ) ;
#2429 = EDGE_CURVE ( 'NONE', #6600, #2463, #1308, .T. ) ;
#2430 = EDGE_CURVE ( 'NONE', #9336, #7089, #4541, .T. ) ;
#2431 = CARTESIAN_POINT ( 'NONE',  ( 39.99999999999997158, -145.1457019118819005, 49.99999999999997868 ) ) ;
#2432 = DIRECTION ( 'NONE',  ( -0.6691306063588580155, -0.7431448254773944662, 0.000000000000000000 ) ) ;
#2433 = CARTESIAN_POINT ( 'NONE',  ( 3.000000000000000000, 0.000000000000000000, 0.000000000000000000 ) ) ;
#2434 = CARTESIAN_POINT ( 'NONE',  ( -16.29350689640809691, -115.1457019118818863, -27.01918567566963247 ) ) ;
#2435 = ORIENTED_EDGE ( 'NONE', *, *, #2550, .F. ) ;
#2436 = AXIS2_PLACEMENT_3D ( 'NONE', #10103, #1245, #7612 ) ;
#2437 = ORIENTED_EDGE ( 'NONE', *, *, #4240, .F. ) ;
#2438 = ORIENTED_EDGE ( 'NONE', *, *, #5905, .T. ) ;
#2439 = VERTEX_POINT ( 'NONE', #5384 ) ;
#2440 = DIRECTION ( 'NONE',  ( 1.000000000000000000, -0.000000000000000000, -0.000000000000000000 ) ) ;
#2441 = DIRECTION ( 'NONE',  ( 0.6691306063588561281, 0.7431448254773961315, 0.000000000000000000 ) ) ;
#2442 = AXIS2_PLACEMENT_3D ( 'NONE', #7793, #6693, #2618 ) ;
#2443 = EDGE_CURVE ( 'NONE', #2136, #6531, #8463, .T. ) ;
#2444 = DIRECTION ( 'NONE',  ( -0.000000000000000000, -0.000000000000000000, 1.000000000000000000 ) ) ;
#2445 = ORIENTED_EDGE ( 'NONE', *, *, #2306, .F. ) ;
#2446 = CARTESIAN_POINT ( 'NONE',  ( -20.29350689640810401, 150.5696653505793563, 10.98204862120179826 ) ) ;
#2447 = ORIENTED_EDGE ( 'NONE', *, *, #3925, .F. ) ;
#2448 = DIRECTION ( 'NONE',  ( 0.000000000000000000, -1.000000000000000000, 0.000000000000000000 ) ) ;
#2449 = EDGE_CURVE ( 'NONE', #9987, #8969, #3678, .T. ) ;
#2450 = AXIS2_PLACEMENT_3D ( 'NONE', #1437, #4811, #791 ) ;
#2451 = VERTEX_POINT ( 'NONE', #9474 ) ;
#2452 = AXIS2_PLACEMENT_3D ( 'NONE', #7846, #10392, #3026 ) ;
#2453 = CARTESIAN_POINT ( 'NONE',  ( -43.93820948810023452, 0.000000000000000000, 0.000000000000000000 ) ) ;
#2454 = PLANE ( 'NONE',  #2246 ) ;
#2455 = CYLINDRICAL_SURFACE ( 'NONE', #3976, 2.000000000000001776 ) ;
#2456 = CARTESIAN_POINT ( 'NONE',  ( 37.46807877396356190, -135.0538248752150139, -26.54476371764646103 ) ) ;
#2457 = ORIENTED_EDGE ( 'NONE', *, *, #4077, .F. ) ;
#2458 = FACE_OUTER_BOUND ( 'NONE', #3220, .T. ) ;
#2459 = CONTEXT_DEPENDENT_SHAPE_REPRESENTATION ( #4566, #1714 ) ;
#2460 = ORIENTED_EDGE ( 'NONE', *, *, #2340, .F. ) ;
#2461 = ADVANCED_FACE ( 'NONE', ( #4390 ), #7622, .F. ) ;
#2462 = CARTESIAN_POINT ( 'NONE',  ( -38.19229777560033057, 152.5696653505793279, -12.50000000000000000 ) ) ;
#2463 = VERTEX_POINT ( 'NONE', #6818 ) ;
#2464 = AXIS2_PLACEMENT_3D ( 'NONE', #935, #8088, #878 ) ;
#2465 = ORIENTED_EDGE ( 'NONE', *, *, #3079, .F. ) ;
#2466 = FACE_BOUND ( 'NONE', #3000, .T. ) ;
#2467 = DIRECTION ( 'NONE',  ( 0.000000000000000000, 0.000000000000000000, -1.000000000000000000 ) ) ;
#2468 = LINE ( 'NONE', #5695, #4671 ) ;
#2469 = AXIS2_PLACEMENT_3D ( 'NONE', #4152, #4935, #5894 ) ;
#2470 = CARTESIAN_POINT ( 'NONE',  ( -18.34874108452141783, -140.1746510883711778, -50.00000000000002132 ) ) ;
#2471 = DIRECTION ( 'NONE',  ( -1.000000000000000000, -1.734723475976805319E-15, -0.000000000000000000 ) ) ;
#2472 = PRODUCT ( 'C-Frame Ductile Iron Housing', 'C-Frame Ductile Iron Housing', '', ( #192 ) ) ;
#2473 = EDGE_CURVE ( 'NONE', #1535, #5197, #7669, .T. ) ;
#2474 = VERTEX_POINT ( 'NONE', #413 ) ;
#2475 = AXIS2_PLACEMENT_3D ( 'NONE', #6834, #3713, #5342 ) ;
#2476 = EDGE_LOOP ( 'NONE', ( #704, #3245, #648, #8165, #2567, #2846, #1417, #1179, #5247, #9908, #8106, #2341 ) ) ;
#2477 = CARTESIAN_POINT ( 'NONE',  ( 14.70649310359190309, 120.5696653505793705, 16.00000000000000711 ) ) ;
#2478 = FACE_OUTER_BOUND ( 'NONE', #3614, .T. ) ;
#2479 = CARTESIAN_POINT ( 'NONE',  ( -7.293506896408097795, 2.445795361565304815E-15, 20.00000000000002132 ) ) ;
#2480 = FACE_OUTER_BOUND ( 'NONE', #8443, .T. ) ;
#2481 = DIRECTION ( 'NONE',  ( 0.000000000000000000, 0.000000000000000000, 1.000000000000000000 ) ) ;
#2482 = DIRECTION ( 'NONE',  ( -0.000000000000000000, 1.329743448921560837E-15, 1.000000000000000000 ) ) ;
#2483 = ORIENTED_EDGE ( 'NONE', *, *, #8314, .F. ) ;
#2484 = AXIS2_PLACEMENT_3D ( 'NONE', #3876, #9546, #7106 ) ;
#2485 = ORIENTED_EDGE ( 'NONE', *, *, #7022, .F. ) ;
#2486 = EDGE_CURVE ( 'NONE', #7639, #9939, #3645, .T. ) ;
#2487 = EDGE_CURVE ( 'NONE', #1403, #5783, #9113, .T. ) ;
#2488 = ORIENTED_EDGE ( 'NONE', *, *, #2547, .F. ) ;
#2489 = EDGE_CURVE ( 'NONE', #2732, #5224, #4039, .T. ) ;
#2490 = TOROIDAL_SURFACE ( 'NONE', #3682, 75.59748767972220662, 70.74985237403969052 ) ;
#2491 = ORIENTED_EDGE ( 'NONE', *, *, #1774, .T. ) ;
#2492 = CARTESIAN_POINT ( 'NONE',  ( -30.29350689640809335, 72.56966535057935630, -20.00000000000001066 ) ) ;
#2493 = DIRECTION ( 'NONE',  ( 0.7431448254773962425, -0.6691306063588559061, 0.000000000000000000 ) ) ;
#2494 = CLOSED_SHELL ( 'NONE', ( #6615, #4121, #6110, #6557, #8776, #2563, #2234, #10016, #9921, #9641, #605, #7555, #2809, #8581, #9569, #6898, #4061, #9141, #8020, #2008, #8104, #10074, #168, #6055, #3671, #6423, #3511, #3092, #5918, #10464, #9230, #5878, #8436, #8217 ) ) ;
#2495 = CARTESIAN_POINT ( 'NONE',  ( 0.000000000000000000, 1.467624384280025174, -2.542000000000001592 ) ) ;
#2496 = CARTESIAN_POINT ( 'NONE',  ( -16.29350689640809691, -19.43033464942062238, 0.000000000000000000 ) ) ;
#2497 = AXIS2_PLACEMENT_3D ( 'NONE', #5723, #9930, #2548 ) ;
#2498 = VERTEX_POINT ( 'NONE', #7141 ) ;
#2499 = CYLINDRICAL_SURFACE ( 'NONE', #5532, 3.000000000000000444 ) ;
#2500 = VERTEX_POINT ( 'NONE', #10423 ) ;
#2501 = DIRECTION ( 'NONE',  ( 0.000000000000000000, 0.000000000000000000, -1.000000000000000000 ) ) ;
#2502 = AXIS2_PLACEMENT_3D ( 'NONE', #7643, #3779, #4518 ) ;
#2503 = EDGE_CURVE ( 'NONE', #5058, #6356, #3028, .T. ) ;
#2504 =( BOUNDED_CURVE ( )  B_SPLINE_CURVE ( 3, ( #1292, #4526, #5900, #9138 ),
 .UNSPECIFIED., .F., .T. ) 
 B_SPLINE_CURVE_WITH_KNOTS ( ( 4, 4 ),
 ( 0.9691135948774319830, 1.037548729184187613 ),
 .UNSPECIFIED. ) 
 CURVE ( )  GEOMETRIC_REPRESENTATION_ITEM ( )  RATIONAL_B_SPLINE_CURVE ( ( 1.000000000000000000, 0.9996097574442918132, 0.9996097574442918132, 1.000000000000000000 ) ) 
 REPRESENTATION_ITEM ( '' )  );
#2505 = ORIENTED_EDGE ( 'NONE', *, *, #5133, .F. ) ;
#2506 = UNCERTAINTY_MEASURE_WITH_UNIT (LENGTH_MEASURE( 1.000000000000000082E-05 ), #6253, 'distance_accuracy_value', 'NONE');
#2507 = DIRECTION ( 'NONE',  ( 1.277197683604454965E-16, -1.000000000000000000, 0.000000000000000000 ) ) ;
#2508 = FACE_BOUND ( 'NONE', #5851, .T. ) ;
#2509 = DIRECTION ( 'NONE',  ( -0.000000000000000000, 1.000000000000000000, -0.000000000000000000 ) ) ;
#2510 = DIRECTION ( 'NONE',  ( 0.000000000000000000, 0.000000000000000000, 1.000000000000000000 ) ) ;
#2511 = VECTOR ( 'NONE', #9492, 1000.000000000000227 ) ;
#2512 = FACE_OUTER_BOUND ( 'NONE', #1164, .T. ) ;
#2513 = CARTESIAN_POINT ( 'NONE',  ( -30.29350689640809335, 2.445795361565304815E-15, 20.00000000000002132 ) ) ;
#2514 = VERTEX_POINT ( 'NONE', #8028 ) ;
#2515 = VECTOR ( 'NONE', #35, 1000.000000000000000 ) ;
#2516 = CARTESIAN_POINT ( 'NONE',  ( -2.293506896408097795, 80.56966535057935630, -16.00000000000000711 ) ) ;
#2517 = ORIENTED_EDGE ( 'NONE', *, *, #3629, .F. ) ;
#2518 = CARTESIAN_POINT ( 'NONE',  ( -27.15769640663941331, -135.1457019118818721, 47.99999999999997868 ) ) ;
#2519 = ORIENTED_EDGE ( 'NONE', *, *, #7483, .F. ) ;
#2520 = CIRCLE ( 'NONE', #4213, 7.999999999999991118 ) ;
#2521 = EDGE_CURVE ( 'NONE', #7666, #264, #4203, .T. ) ;
#2522 = FACE_BOUND ( 'NONE', #7412, .T. ) ;
#2523 = DIRECTION ( 'NONE',  ( -1.000000000000000000, 0.000000000000000000, 0.000000000000000000 ) ) ;
#2524 = CARTESIAN_POINT ( 'NONE',  ( 14.70649310359190309, 120.5696653505793705, 24.00000000000000711 ) ) ;
#2525 = DIRECTION ( 'NONE',  ( 0.000000000000000000, -1.000000000000000000, 0.000000000000000000 ) ) ;
#2526 = CARTESIAN_POINT ( 'NONE',  ( 5.999999999999998224, 0.000000000000000000, 0.000000000000000000 ) ) ;
#2527 = VECTOR ( 'NONE', #1208, 1000.000000000000000 ) ;
#2528 = EDGE_LOOP ( 'NONE', ( #771, #5503, #4451, #7777, #2730, #8563 ) ) ;
#2529 = DIRECTION ( 'NONE',  ( 0.000000000000000000, -1.000000000000000000, 1.222897680782651224E-16 ) ) ;
#2530 = ORIENTED_EDGE ( 'NONE', *, *, #5258, .T. ) ;
#2531 = DIRECTION ( 'NONE',  ( 7.848480207562752404E-17, -1.000000000000000000, -7.143558635763577733E-33 ) ) ;
#2532 = FACE_BOUND ( 'NONE', #361, .T. ) ;
#2533 = CARTESIAN_POINT ( 'NONE',  ( -47.94539818030330025, 150.5446653505793790, 0.000000000000000000 ) ) ;
#2534 = DIRECTION ( 'NONE',  ( 1.000000000000000000, 0.000000000000000000, 0.000000000000000000 ) ) ;
#2535 = ADVANCED_FACE ( 'NONE', ( #4010 ), #6436, .T. ) ;
#2536 = DIRECTION ( 'NONE',  ( 0.000000000000000000, 0.000000000000000000, 1.000000000000000000 ) ) ;
#2537 = CARTESIAN_POINT ( 'NONE',  ( 18.34874108452142494, -140.1746510883711778, 49.99999999999997868 ) ) ;
#2538 = EDGE_LOOP ( 'NONE', ( #273, #1647, #3485, #1189 ) ) ;
#2539 = ORIENTED_EDGE ( 'NONE', *, *, #4294, .T. ) ;
#2540 = ORIENTED_EDGE ( 'NONE', *, *, #6007, .F. ) ;
#2541 = EDGE_LOOP ( 'NONE', ( #2097, #5873, #6376, #4643 ) ) ;
#2542 = VERTEX_POINT ( 'NONE', #7190 ) ;
#2543 = CARTESIAN_POINT ( 'NONE',  ( -30.29350689640809335, 120.5696653505793705, 24.00000000000000711 ) ) ;
#2544 = DIRECTION ( 'NONE',  ( -0.000000000000000000, -0.000000000000000000, -1.000000000000000000 ) ) ;
#2545 = ORIENTED_EDGE ( 'NONE', *, *, #4863, .T. ) ;
#2546 = CARTESIAN_POINT ( 'NONE',  ( 39.99999999999997158, -135.1457019118818721, 39.99999999999997868 ) ) ;
#2547 = EDGE_CURVE ( 'NONE', #9480, #6361, #10475, .T. ) ;
#2548 = DIRECTION ( 'NONE',  ( 0.000000000000000000, 0.000000000000000000, -1.000000000000000000 ) ) ;
#2549 = EDGE_CURVE ( 'NONE', #4432, #3359, #721, .T. ) ;
#2550 = EDGE_CURVE ( 'NONE', #4450, #2362, #7596, .T. ) ;
#2551 = VERTEX_POINT ( 'NONE', #10325 ) ;
#2552 = CYLINDRICAL_SURFACE ( 'NONE', #4180, 3.999999999999989786 ) ;
#2553 = VERTEX_POINT ( 'NONE', #8082 ) ;
#2554 = CARTESIAN_POINT ( 'NONE',  ( -20.29350689640810046, 150.5696653505793563, -20.00000000000000355 ) ) ;
#2555 = ORIENTED_EDGE ( 'NONE', *, *, #8994, .T. ) ;
#2556 = CIRCLE ( 'NONE', #6440, 1.999999999999998224 ) ;
#2557 = ORIENTED_EDGE ( 'NONE', *, *, #6529, .T. ) ;
#2558 = CARTESIAN_POINT ( 'NONE',  ( -39.00000000000000000, -3.117691453623975484, -1.800000000000017586 ) ) ;
#2559 = FILL_AREA_STYLE_COLOUR ( '', #8820 ) ;
#2560 = CARTESIAN_POINT ( 'NONE',  ( 17.97972049165455388, 17.84145331825995484, -25.00000000000000355 ) ) ;
#2561 = DIRECTION ( 'NONE',  ( -1.396588258780021135E-16, 0.000000000000000000, -1.000000000000000000 ) ) ;
#2562 = EDGE_CURVE ( 'NONE', #9948, #9616, #9283, .T. ) ;
#2563 = ADVANCED_FACE ( 'NONE', ( #4644 ), #3208, .F. ) ;
#2564 = CARTESIAN_POINT ( 'NONE',  ( -27.15769640663941331, -133.1457019118818721, -1.896405996851248439E-14 ) ) ;
#2565 = CARTESIAN_POINT ( 'NONE',  ( -40.00000000000001421, -135.1457019118818721, -40.00000000000002132 ) ) ;
#2566 = AXIS2_PLACEMENT_3D ( 'NONE', #9000, #786, #5706 ) ;
#2567 = ORIENTED_EDGE ( 'NONE', *, *, #5846, .T. ) ;
#2568 = AXIS2_PLACEMENT_3D ( 'NONE', #5305, #10248, #6908 ) ;
#2569 = CARTESIAN_POINT ( 'NONE',  ( 23.15769640663936002, -115.1457019118818863, -3.234176690190481738E-15 ) ) ;
#2570 = CONTEXT_DEPENDENT_SHAPE_REPRESENTATION ( #1321, #779 ) ;
#2571 = ORIENTED_EDGE ( 'NONE', *, *, #9829, .T. ) ;
#2572 = CARTESIAN_POINT ( 'NONE',  ( -26.27514770175547199, -135.1457019118818721, 49.99999999999998579 ) ) ;
#2573 = ORIENTED_EDGE ( 'NONE', *, *, #7, .T. ) ;
#2574 = AXIS2_PLACEMENT_3D ( 'NONE', #6824, #8307, #3595 ) ;
#2575 = AXIS2_PLACEMENT_3D ( 'NONE', #8320, #4873, #7320 ) ;
#2576 = DIRECTION ( 'NONE',  ( -0.000000000000000000, 1.000000000000000000, -0.000000000000000000 ) ) ;
#2577 = DIRECTION ( 'NONE',  ( 0.000000000000000000, 0.000000000000000000, -1.000000000000000000 ) ) ;
#2578 = CARTESIAN_POINT ( 'NONE',  ( -23.15769640663937423, -133.1457019118818721, -48.00000000000002132 ) ) ;
#2579 = CARTESIAN_POINT ( 'NONE',  ( -40.00000000000002842, -135.1457019118818721, 43.99999999999997158 ) ) ;
#2580 = LINE ( 'NONE', #9855, #6127 ) ;
#2581 = AXIS2_PLACEMENT_3D ( 'NONE', #3988, #4678, #8705 ) ;
#2582 = CIRCLE ( 'NONE', #4777, 4.000000000000000000 ) ;
#2583 = EDGE_CURVE ( 'NONE', #3341, #9180, #5721, .T. ) ;
#2584 = ORIENTED_EDGE ( 'NONE', *, *, #3629, .T. ) ;
#2585 = CARTESIAN_POINT ( 'NONE',  ( -54.56278605312611774, 170.3918540369290895, 0.000000000000000000 ) ) ;
#2586 = VERTEX_POINT ( 'NONE', #8877 ) ;
#2587 = CARTESIAN_POINT ( 'NONE',  ( 53.40242741783141156, 52.77167129626698028, -30.00000000000000355 ) ) ;
#2588 = LINE ( 'NONE', #4232, #3413 ) ;
#2589 = CONICAL_SURFACE ( 'NONE', #6826, 2.541999999999999815, 1.047197551196591858 ) ;
#2590 = EDGE_LOOP ( 'NONE', ( #6199, #5120, #6180, #2437, #4980, #9978 ) ) ;
#2591 = CARTESIAN_POINT ( 'NONE',  ( -16.29350689640809691, 105.5289575273812233, -7.749999999999996447 ) ) ;
#2592 = CARTESIAN_POINT ( 'NONE',  ( -16.29350689640809691, 105.5289575273812233, -25.04213562373096380 ) ) ;
#2593 = AXIS2_PLACEMENT_3D ( 'NONE', #5648, #6444, #9694 ) ;
#2594 = DIRECTION ( 'NONE',  ( 0.07334937666141724821, -0.9973063064792989652, -0.000000000000000000 ) ) ;
#2595 = CARTESIAN_POINT ( 'NONE',  ( -0.8557715602033003632, -6.505213034913026604E-16, 3.600000000000000977 ) ) ;
#2596 = VERTEX_POINT ( 'NONE', #9531 ) ;
#2597 = ORIENTED_EDGE ( 'NONE', *, *, #8641, .F. ) ;
#2598 = ORIENTED_EDGE ( 'NONE', *, *, #7222, .F. ) ;
#2599 = CARTESIAN_POINT ( 'NONE',  ( -16.29350689640809691, -8.660287962196477451, 0.000000000000000000 ) ) ;
#2600 = FACE_OUTER_BOUND ( 'NONE', #4884, .T. ) ;
#2601 = FACE_OUTER_BOUND ( 'NONE', #5744, .T. ) ;
#2602 = CARTESIAN_POINT ( 'NONE',  ( -117.0000000000000000, 0.2735269159956686957, 3.990636919869546606 ) ) ;
#2603 = AXIS2_PLACEMENT_3D ( 'NONE', #8731, #7100, #9647 ) ;
#2604 = ORIENTED_EDGE ( 'NONE', *, *, #9461, .T. ) ;
#2605 = CARTESIAN_POINT ( 'NONE',  ( -48.00000000000002132, -133.1457019118818721, -25.15769640663945950 ) ) ;
#2606 = AXIS2_PLACEMENT_3D ( 'NONE', #314, #3541, #6766 ) ;
#2607 = ORIENTED_EDGE ( 'NONE', *, *, #9637, .F. ) ;
#2608 = LINE ( 'NONE', #5832, #6751 ) ;
#2609 = EDGE_CURVE ( 'NONE', #4517, #4542, #1165, .T. ) ;
#2610 = AXIS2_PLACEMENT_3D ( 'NONE', #9199, #6758, #9309 ) ;
#2611 = ORIENTED_EDGE ( 'NONE', *, *, #2371, .F. ) ;
#2612 = PRODUCT_DEFINITION_CONTEXT ( 'detailed design', #9516, 'design' ) ;
#2613 = ORIENTED_EDGE ( 'NONE', *, *, #846, .F. ) ;
#2614 = DIRECTION ( 'NONE',  ( -6.982941293900105430E-16, 0.000000000000000000, 1.000000000000000000 ) ) ;
#2615 = PLANE ( 'NONE',  #10186 ) ;
#2616 = DIRECTION ( 'NONE',  ( 0.000000000000000000, -1.000000000000000000, 0.000000000000000000 ) ) ;
#2617 = CARTESIAN_POINT ( 'NONE',  ( 0.000000000000000000, -133.1457019118818721, 25.15769640663938134 ) ) ;
#2618 = DIRECTION ( 'NONE',  ( 0.000000000000000000, -0.000000000000000000, -1.000000000000000000 ) ) ;
#2619 = CARTESIAN_POINT ( 'NONE',  ( 37.71464122736490054, -135.1457019118818721, -27.15769640663940265 ) ) ;
#2620 = VECTOR ( 'NONE', #7443, 1000.000000000000000 ) ;
#2621 = VERTEX_POINT ( 'NONE', #4059 ) ;
#2622 = LINE ( 'NONE', #9897, #2410 ) ;
#2623 = B_SPLINE_CURVE_WITH_KNOTS ( 'NONE', 3,
 ( #2619, #3368, #9730, #5842, #2456, #8021, #4003, #2403, #1612, #819, #4055, #9136, #2716, #346, #5897, #6856 ),
 .UNSPECIFIED., .F., .F.,
 ( 4, 2, 2, 2, 2, 2, 2, 4 ),
 ( 0.000000000000000000, 0.0003992569680943842936, 0.0007985139361887685873, 0.001197770904283152827, 0.001597027872377537175, 0.002395541808566243203, 0.002794798776660634924, 0.003194055744755026210 ),
 .UNSPECIFIED. ) ;
#2624 = AXIS2_PLACEMENT_3D ( 'NONE', #2645, #4074, #5076 ) ;
#2625 = EDGE_CURVE ( 'NONE', #8577, #6600, #5559, .T. ) ;
#2627 = EDGE_CURVE ( 'NONE', #9462, #5715, #6060, .T. ) ;
#2626 = ORIENTED_EDGE ( 'NONE', *, *, #9305, .F. ) ;
#2628 = ADVANCED_FACE ( 'NONE', ( #6489 ), #3960, .F. ) ;
#2629 = DIRECTION ( 'NONE',  ( 0.000000000000000000, -0.000000000000000000, -1.000000000000000000 ) ) ;
#2630 = VERTEX_POINT ( 'NONE', #823 ) ;
#2631 = CIRCLE ( 'NONE', #4821, 2.000000000000001776 ) ;
#2632 = DIRECTION ( 'NONE',  ( -1.000000000000000000, 0.000000000000000000, 0.000000000000000000 ) ) ;
#2633 = DIRECTION ( 'NONE',  ( 1.000000000000000000, 0.000000000000000000, 0.000000000000000000 ) ) ;
#2634 = CARTESIAN_POINT ( 'NONE',  ( 39.99999999999998579, -135.1457019118818721, -40.00000000000002132 ) ) ;
#2635 = LINE ( 'NONE', #2579, #9509 ) ;
#2636 = DIRECTION ( 'NONE',  ( 0.000000000000000000, 0.000000000000000000, 1.000000000000000000 ) ) ;
#2637 = ORIENTED_EDGE ( 'NONE', *, *, #6913, .F. ) ;
#2638 = AXIS2_PLACEMENT_3D ( 'NONE', #3741, #7086, #6975 ) ;
#2639 = EDGE_CURVE ( 'NONE', #3419, #623, #7291, .T. ) ;
#2640 = DIRECTION ( 'NONE',  ( -0.000000000000000000, -0.000000000000000000, 1.000000000000000000 ) ) ;
#2641 = ORIENTED_EDGE ( 'NONE', *, *, #3330, .F. ) ;
#2642 = CARTESIAN_POINT ( 'NONE',  ( -3.173844575093148990, 130.5696653505793847, 10.90000000000000036 ) ) ;
#2643 = DIRECTION ( 'NONE',  ( 0.08084652178105143638, 0.5716988695978858503, 0.8164706010729385621 ) ) ;
#2644 = CARTESIAN_POINT ( 'NONE',  ( 4.856471286862176662, 145.0444252872335937, -30.00000000000000355 ) ) ;
#2645 = CARTESIAN_POINT ( 'NONE',  ( -56.34457570605425758, 137.0132282531173473, 0.000000000000000000 ) ) ;
#2646 = AXIS2_PLACEMENT_3D ( 'NONE', #4728, #2297, #7074 ) ;
#2647 = CARTESIAN_POINT ( 'NONE',  ( -23.79350689640809691, 120.5289575273812233, -7.750000000000000000 ) ) ;
#2648 = ORIENTED_EDGE ( 'NONE', *, *, #3265, .T. ) ;
#2649 = CIRCLE ( 'NONE', #7896, 7.999999999999996447 ) ;
#2650 = CIRCLE ( 'NONE', #6207, 70.74985237403969052 ) ;
#2651 = ORIENTED_EDGE ( 'NONE', *, *, #2153, .F. ) ;
#2652 = CARTESIAN_POINT ( 'NONE',  ( 25.15769640663938134, -133.1457019118818721, -27.15769640663941331 ) ) ;
#2653 = CARTESIAN_POINT ( 'NONE',  ( -1.071796769724492338, 0.000000000000000000, 0.000000000000000000 ) ) ;
#2654 = EDGE_CURVE ( 'NONE', #1005, #4437, #6401, .T. ) ;
#2655 = CARTESIAN_POINT ( 'NONE',  ( -24.31850689640809549, 140.5696653505793563, 7.750000000000002665 ) ) ;
#2656 = AXIS2_PLACEMENT_3D ( 'NONE', #10388, #6352, #5604 ) ;
#2657 = EDGE_LOOP ( 'NONE', ( #1801, #3906 ) ) ;
#2658 = DIRECTION ( 'NONE',  ( -1.000000000000000000, 0.000000000000000000, 0.000000000000000000 ) ) ;
#2659 = EDGE_LOOP ( 'NONE', ( #4320, #7425, #4589, #2248, #9197 ) ) ;
#2660 = CIRCLE ( 'NONE', #4019, 24.24539146688411861 ) ;
#2661 = DIRECTION ( 'NONE',  ( 0.000000000000000000, 0.000000000000000000, 1.000000000000000000 ) ) ;
#2662 = AXIS2_PLACEMENT_3D ( 'NONE', #351, #6805, #2776 ) ;
#2663 = VERTEX_POINT ( 'NONE', #5690 ) ;
#2664 = FILL_AREA_STYLE ('',( #2559 ) ) ;
#2665 = CIRCLE ( 'NONE', #7239, 4.000000000000000000 ) ;
#2666 = CARTESIAN_POINT ( 'NONE',  ( 17.97972049165455388, 37.08684478514406635, 30.00000000000000355 ) ) ;
#2667 = LINE ( 'NONE', #6641, #1559 ) ;
#2668 = PLANE ( 'NONE',  #8879 ) ;
#2669 = EDGE_CURVE ( 'NONE', #1563, #389, #5043, .T. ) ;
#2670 = CARTESIAN_POINT ( 'NONE',  ( 3.000000000000000000, 2.201436576420041202, -1.271000000000003016 ) ) ;
#2671 = CIRCLE ( 'NONE', #651, 2.515249034521771510 ) ;
#2672 = ORIENTED_EDGE ( 'NONE', *, *, #9639, .F. ) ;
#2673 = CARTESIAN_POINT ( 'NONE',  ( 42.22511195853866894, 17.84145331825995839, -30.00000000000000355 ) ) ;
#2674 = ORIENTED_EDGE ( 'NONE', *, *, #2032, .F. ) ;
#2675 = CARTESIAN_POINT ( 'NONE',  ( -27.15769640663937778, -135.1457019118818721, -48.00000000000002132 ) ) ;
#2676 = ORIENTED_EDGE ( 'NONE', *, *, #7129, .F. ) ;
#2677 = VECTOR ( 'NONE', #2531, 1000.000000000000000 ) ;
#2678 = DIRECTION ( 'NONE',  ( 1.000000000000000000, 0.000000000000000000, 0.000000000000000000 ) ) ;
#2679 = AXIS2_PLACEMENT_3D ( 'NONE', #621, #2409, #3157 ) ;
#2680 = DIRECTION ( 'NONE',  ( -0.000000000000000000, 1.000000000000000000, -0.000000000000000000 ) ) ;
#2681 = EDGE_CURVE ( 'NONE', #6001, #9740, #4395, .T. ) ;
#2682 = EDGE_CURVE ( 'NONE', #8294, #3699, #9953, .T. ) ;
#2683 = CARTESIAN_POINT ( 'NONE',  ( -23.17384457509314899, 150.5696653505793563, 10.90000000000000036 ) ) ;
#2684 = EDGE_CURVE ( 'NONE', #9349, #10166, #9982, .T. ) ;
#2685 = DIRECTION ( 'NONE',  ( -1.000000000000000000, 0.000000000000000000, 0.000000000000000000 ) ) ;
#2686 = DIRECTION ( 'NONE',  ( -0.7071067811863512853, 0.000000000000000000, 0.7071067811867437491 ) ) ;
#2687 = ORIENTED_EDGE ( 'NONE', *, *, #9950, .F. ) ;
#2688 = DIRECTION ( 'NONE',  ( -0.6691306063588561281, -0.7431448254773961315, 0.000000000000000000 ) ) ;
#2689 = CIRCLE ( 'NONE', #8275, 7.499999999999996447 ) ;
#2690 = ORIENTED_EDGE ( 'NONE', *, *, #9935, .T. ) ;
#2691 = CARTESIAN_POINT ( 'NONE',  ( -25.15769640663940621, -117.1457019118819005, 27.15769640663938489 ) ) ;
#2692 = CARTESIAN_POINT ( 'NONE',  ( -48.00000000000002132, -133.1457019118818721, 27.15769640663938489 ) ) ;
#2693 = DIRECTION ( 'NONE',  ( -0.9973063064792990762, -0.07334937666141726209, 0.000000000000000000 ) ) ;
#2694 = CARTESIAN_POINT ( 'NONE',  ( 39.99999999999997158, -135.1457019118818721, 39.99999999999997868 ) ) ;
#2695 = CARTESIAN_POINT ( 'NONE',  ( -11.29350689640809158, 105.5289575273812233, -7.749999999999997335 ) ) ;
#2696 = EDGE_CURVE ( 'NONE', #5111, #5490, #5902, .T. ) ;
#2697 = DIRECTION ( 'NONE',  ( -0.000000000000000000, 1.000000000000000000, -0.000000000000000000 ) ) ;
#2698 = VERTEX_POINT ( 'NONE', #7450 ) ;
#2699 = VERTEX_POINT ( 'NONE', #3312 ) ;
#2700 = CARTESIAN_POINT ( 'NONE',  ( 94.78677303995212355, -145.1457019118819005, -30.00000000000000355 ) ) ;
#2701 = DIRECTION ( 'NONE',  ( -0.000000000000000000, -1.000000000000000000, -0.000000000000000000 ) ) ;
#2702 = CARTESIAN_POINT ( 'NONE',  ( 4.856471286862175774, 152.5696653505793279, 30.00000000000000355 ) ) ;
#2703 = CARTESIAN_POINT ( 'NONE',  ( -141.9789400531797412, 249.1017126355397977, 0.000000000000000000 ) ) ;
#2704 = ORIENTED_EDGE ( 'NONE', *, *, #9568, .T. ) ;
#2705 = CARTESIAN_POINT ( 'NONE',  ( -16.29350689640809691, -19.43033464942062238, -7.500000000000000000 ) ) ;
#2706 = ORIENTED_EDGE ( 'NONE', *, *, #8541, .T. ) ;
#2707 = FACE_OUTER_BOUND ( 'NONE', #7118, .T. ) ;
#2708 = EDGE_CURVE ( 'NONE', #8577, #1967, #248, .T. ) ;
#2709 = VERTEX_POINT ( 'NONE', #9040 ) ;
#2710 = EDGE_LOOP ( 'NONE', ( #9393, #4163, #9139, #4148 ) ) ;
#2711 = DIRECTION ( 'NONE',  ( 1.000000000000000000, 0.000000000000000000, 0.000000000000000000 ) ) ;
#2712 = FACE_OUTER_BOUND ( 'NONE', #796, .T. ) ;
#2713 = FACE_OUTER_BOUND ( 'NONE', #2710, .T. ) ;
#2714 = FACE_OUTER_BOUND ( 'NONE', #8892, .T. ) ;
#2715 = DIRECTION ( 'NONE',  ( 0.000000000000000000, 0.000000000000000000, -1.000000000000000000 ) ) ;
#2716 = CARTESIAN_POINT ( 'NONE',  ( 37.23009335863751801, -133.6763800654832153, -25.22473604584575924 ) ) ;
#2717 = ORIENTED_EDGE ( 'NONE', *, *, #2340, .T. ) ;
#2718 = CARTESIAN_POINT ( 'NONE',  ( 39.99999999999997158, -135.1457019118818721, 35.99999999999999289 ) ) ;
#2719 = COLOUR_RGB ( '',0.7921568627450980005, 0.8196078431372548767, 0.9333333333333333481 ) ;
#2720 = ORIENTED_EDGE ( 'NONE', *, *, #4427, .T. ) ;
#2721 = FACE_OUTER_BOUND ( 'NONE', #6822, .T. ) ;
#2722 = EDGE_CURVE ( 'NONE', #10235, #991, #5056, .T. ) ;
#2723 = VERTEX_POINT ( 'NONE', #2518 ) ;
#2724 =( NAMED_UNIT ( * ) PLANE_ANGLE_UNIT ( ) SI_UNIT ( $, .RADIAN. ) );
#2725 = AXIS2_PLACEMENT_3D ( 'NONE', #1412, #4640, #7088 ) ;
#2726 = DIRECTION ( 'NONE',  ( -1.000000000000000000, -0.000000000000000000, -0.000000000000000000 ) ) ;
#2727 = PRESENTATION_LAYER_ASSIGNMENT (  '', '', ( #866 ) ) ;
#2728 = CARTESIAN_POINT ( 'NONE',  ( -25.15769640663940621, -133.1457019118818721, 27.15769640663938489 ) ) ;
#2729 = DIRECTION ( 'NONE',  ( -1.000000000000000000, -0.000000000000000000, -0.000000000000000000 ) ) ;
#2730 = ORIENTED_EDGE ( 'NONE', *, *, #4878, .F. ) ;
#2731 = DIRECTION ( 'NONE',  ( -0.000000000000000000, 1.000000000000000000, 0.000000000000000000 ) ) ;
#2732 = VERTEX_POINT ( 'NONE', #5800 ) ;
#2733 = ORIENTED_EDGE ( 'NONE', *, *, #5857, .F. ) ;
#2734 = AXIS2_PLACEMENT_3D ( 'NONE', #3821, #642, #9493 ) ;
#2735 = DIRECTION ( 'NONE',  ( 0.000000000000000000, 0.3481865296036273372, 0.9374252720097653313 ) ) ;
#2736 = VECTOR ( 'NONE', #3558, 1000.000000000000000 ) ;
#2737 = ADVANCED_FACE ( 'NONE', ( #9140 ), #4112, .T. ) ;
#2738 = ADVANCED_FACE ( 'NONE', ( #5743, #1879 ), #1723, .F. ) ;
#2739 = VERTEX_POINT ( 'NONE', #3420 ) ;
#2740 = FACE_OUTER_BOUND ( 'NONE', #260, .T. ) ;
#2741 = DIRECTION ( 'NONE',  ( 0.000000000000000000, 0.000000000000000000, 1.000000000000000000 ) ) ;
#2742 = LINE ( 'NONE', #3598, #8452 ) ;
#2743 = CARTESIAN_POINT ( 'NONE',  ( -30.29350689640809335, 88.56966535057934209, 20.00000000000001066 ) ) ;
#2744 = CARTESIAN_POINT ( 'NONE',  ( -126.8992195029584025, 225.1284128614458950, 0.000000000000000000 ) ) ;
#2745 = AXIS2_PLACEMENT_3D ( 'NONE', #8570, #2211, #7779 ) ;
#2746 = CARTESIAN_POINT ( 'NONE',  ( -39.65557114539780059, -3.552635616211478720, -1.840410121656805620 ) ) ;
#2747 = AXIS2_PLACEMENT_3D ( 'NONE', #4484, #6070, #10007 ) ;
#2748 = ORIENTED_EDGE ( 'NONE', *, *, #6572, .T. ) ;
#2749 = ORIENTED_EDGE ( 'NONE', *, *, #1233, .F. ) ;
#2750 = ADVANCED_FACE ( 'NONE', ( #9901 ), #3472, .F. ) ;
#2751 = EDGE_CURVE ( 'NONE', #5926, #4123, #5899, .T. ) ;
#2752 = CIRCLE ( 'NONE', #889, 7.785108809001807906 ) ;
#2753 = ADVANCED_FACE ( 'NONE', ( #1828 ), #926, .T. ) ;
#2754 = AXIS2_PLACEMENT_3D ( 'NONE', #8874, #9084, #8289 ) ;
#2755 = CARTESIAN_POINT ( 'NONE',  ( 39.99999999999998579, -135.1457019118818721, -35.97500000000002274 ) ) ;
#2756 = DIRECTION ( 'NONE',  ( -1.000000000000000000, -1.802741689055041147E-15, 0.000000000000000000 ) ) ;
#2757 = DIRECTION ( 'NONE',  ( 0.000000000000000000, 0.000000000000000000, -1.000000000000000000 ) ) ;
#2758 = ORIENTED_EDGE ( 'NONE', *, *, #6627, .T. ) ;
#2759 = ORIENTED_EDGE ( 'NONE', *, *, #332, .T. ) ;
#2760 = CARTESIAN_POINT ( 'NONE',  ( -47.94539818030330025, 150.5696653505793563, 0.000000000000000000 ) ) ;
#2761 = ORIENTED_EDGE ( 'NONE', *, *, #259, .F. ) ;
#2762 = EDGE_CURVE ( 'NONE', #3747, #9349, #7552, .T. ) ;
#2763 = LINE ( 'NONE', #1917, #10462 ) ;
#2764 = LINE ( 'NONE', #9236, #5097 ) ;
#2765 = CIRCLE ( 'NONE', #6833, 3.999999999999996447 ) ;
#2766 = DIRECTION ( 'NONE',  ( 0.000000000000000000, 0.000000000000000000, 1.000000000000000000 ) ) ;
#2767 = FACE_OUTER_BOUND ( 'NONE', #347, .T. ) ;
#2768 = EDGE_CURVE ( 'NONE', #4517, #4943, #9289, .T. ) ;
#2769 = DIRECTION ( 'NONE',  ( -0.000000000000000000, 1.000000000000000000, -0.000000000000000000 ) ) ;
#2770 = ORIENTED_EDGE ( 'NONE', *, *, #7364, .F. ) ;
#2771 = CARTESIAN_POINT ( 'NONE',  ( -38.19229777560033057, 37.08684478514405214, 12.50000000000000000 ) ) ;
#2772 = CIRCLE ( 'NONE', #8702, 26.17065043502059396 ) ;
#2773 = ORIENTED_EDGE ( 'NONE', *, *, #9575, .F. ) ;
#2774 = PRODUCT_DEFINITION_FORMATION_WITH_SPECIFIED_SOURCE ( 'ANY', '', #5424, .NOT_KNOWN. ) ;
#2775 = DIRECTION ( 'NONE',  ( -1.000000000000000000, 0.000000000000000000, 0.000000000000000000 ) ) ;
#2776 = DIRECTION ( 'NONE',  ( 0.000000000000000000, 0.000000000000000000, 1.000000000000000000 ) ) ;
#2777 = AXIS2_PLACEMENT_3D ( 'NONE', #3046, #7085, #2199 ) ;
#2778 = CARTESIAN_POINT ( 'NONE',  ( 37.71464122736488633, -135.1457019118818721, 27.15769640663938489 ) ) ;
#2779 = ADVANCED_FACE ( 'NONE', ( #2721 ), #5394, .F. ) ;
#2780 = CARTESIAN_POINT ( 'NONE',  ( 25.15769640663936357, -117.1457019118819005, 27.15769640663938489 ) ) ;
#2781 = DIRECTION ( 'NONE',  ( -0.000000000000000000, -1.000000000000000000, -0.000000000000000000 ) ) ;
#2782 = ORIENTED_EDGE ( 'NONE', *, *, #2264, .F. ) ;
#2783 = CARTESIAN_POINT ( 'NONE',  ( 14.70649310359190309, 120.5696653505793705, -16.00000000000000711 ) ) ;
#2784 = VERTEX_POINT ( 'NONE', #350 ) ;
#2785 = DIRECTION ( 'NONE',  ( 0.000000000000000000, 0.000000000000000000, 1.000000000000000000 ) ) ;
#2786 = ORIENTED_EDGE ( 'NONE', *, *, #10087, .T. ) ;
#2787 = DIRECTION ( 'NONE',  ( 1.000000000000000000, 0.000000000000000000, -0.000000000000000000 ) ) ;
#2788 = AXIS2_PLACEMENT_3D ( 'NONE', #4184, #7417, #3388 ) ;
#2789 = ORIENTED_EDGE ( 'NONE', *, *, #5653, .T. ) ;
#2790 = LINE ( 'NONE', #4393, #5178 ) ;
#2791 = DIRECTION ( 'NONE',  ( 0.000000000000000000, -0.9374252720097652203, -0.3481865296036273372 ) ) ;
#2792 = LINE ( 'NONE', #10017, #2527 ) ;
#2793 = CARTESIAN_POINT ( 'NONE',  ( -50.00000000000002842, -145.1457019118819005, 39.99999999999997868 ) ) ;
#2794 = DIRECTION ( 'NONE',  ( -0.000000000000000000, 1.000000000000000000, -0.000000000000000000 ) ) ;
#2795 = DIRECTION ( 'NONE',  ( 0.000000000000000000, 0.000000000000000000, 1.000000000000000000 ) ) ;
#2796 = ADVANCED_FACE ( 'NONE', ( #6803 ), #1170, .F. ) ;
#2797 = CIRCLE ( 'NONE', #4157, 3.000000000000000444 ) ;
#2798 = EDGE_LOOP ( 'NONE', ( #10043, #9182, #5890, #1464 ) ) ;
#2799 = EDGE_LOOP ( 'NONE', ( #8482, #7532, #663 ) ) ;
#2800 = DIRECTION ( 'NONE',  ( 0.000000000000000000, -0.5000000000000012212, -0.8660254037844380415 ) ) ;
#2801 = CIRCLE ( 'NONE', #2983, 5.000000000000000888 ) ;
#2802 = ORIENTED_EDGE ( 'NONE', *, *, #2883, .T. ) ;
#2803 = DIRECTION ( 'NONE',  ( -1.000000000000000000, 0.000000000000000000, 0.000000000000000000 ) ) ;
#2804 = VECTOR ( 'NONE', #4535, 1000.000000000000000 ) ;
#2805 = CARTESIAN_POINT ( 'NONE',  ( -40.99999999999999289, -3.464101615137750834, -2.000000000000019096 ) ) ;
#2806 = DIRECTION ( 'NONE',  ( 0.000000000000000000, 0.000000000000000000, -1.000000000000000000 ) ) ;
#2807 = EDGE_LOOP ( 'NONE', ( #1841, #3283, #8792, #3496 ) ) ;
#2808 = EDGE_CURVE ( 'NONE', #941, #9176, #7767, .T. ) ;
#2809 = ADVANCED_FACE ( 'NONE', ( #4376 ), #5951, .F. ) ;
#2810 = AXIS2_PLACEMENT_3D ( 'NONE', #2981, #8549, #8601 ) ;
#2811 = ADVANCED_FACE ( 'NONE', ( #6966 ), #7707, .T. ) ;
#2812 = ORIENTED_EDGE ( 'NONE', *, *, #3269, .T. ) ;
#2813 =( LENGTH_UNIT ( ) NAMED_UNIT ( * ) SI_UNIT ( .MILLI., .METRE. ) );
#2814 = CIRCLE ( 'NONE', #2646, 1.999999999999998224 ) ;
#2815 = VERTEX_POINT ( 'NONE', #5161 ) ;
#2816 = ORIENTED_EDGE ( 'NONE', *, *, #2872, .T. ) ;
#2817 = CARTESIAN_POINT ( 'NONE',  ( -21.29350689640810401, 105.5289575273812233, -7.749999999999999112 ) ) ;
#2818 = PLANE ( 'NONE',  #7976 ) ;
#2819 = AXIS2_PLACEMENT_3D ( 'NONE', #157, #992, #3382 ) ;
#2820 = CARTESIAN_POINT ( 'NONE',  ( 73.53765631853929108, 70.39106037767953694, 25.00000000000000000 ) ) ;
#2821 = DIRECTION ( 'NONE',  ( 0.000000000000000000, 0.000000000000000000, 1.000000000000000000 ) ) ;
#2822 = CIRCLE ( 'NONE', #9606, 20.00000000000000000 ) ;
#2823 = AXIS2_PLACEMENT_3D ( 'NONE', #5003, #1676, #827 ) ;
#2824 = CARTESIAN_POINT ( 'NONE',  ( -23.48622939173161228, -144.8896666241527669, 3.853145670227867470 ) ) ;
#2825 = ADVANCED_FACE ( 'NONE', ( #9353 ), #9403, .F. ) ;
#2826 = ORIENTED_EDGE ( 'NONE', *, *, #3953, .T. ) ;
#2827 = DIRECTION ( 'NONE',  ( -0.000000000000000000, 0.000000000000000000, -1.000000000000000000 ) ) ;
#2828 = VECTOR ( 'NONE', #1708, 1000.000000000000000 ) ;
#2829 = DIRECTION ( 'NONE',  ( -0.6691306063588566833, -0.7431448254773957984, 0.000000000000000000 ) ) ;
#2830 = CIRCLE ( 'NONE', #2497, 4.000000000000000000 ) ;
#2831 = CARTESIAN_POINT ( 'NONE',  ( 27.15769640663935647, -135.1457019118818721, 2.654968395591742513E-14 ) ) ;
#2832 = CIRCLE ( 'NONE', #8766, 3.999999999999976019 ) ;
#2833 = CARTESIAN_POINT ( 'NONE',  ( -37.01000625782472753, 0.000000000000000000, 0.000000000000000000 ) ) ;
#2834 = CARTESIAN_POINT ( 'NONE',  ( 37.23183231822027750, -133.8039134404564265, 25.26438245347419809 ) ) ;
#2835 = DIRECTION ( 'NONE',  ( 0.000000000000000000, 0.000000000000000000, 1.000000000000000000 ) ) ;
#2836 = DIRECTION ( 'NONE',  ( 0.000000000000000000, 0.000000000000000000, -1.000000000000000000 ) ) ;
#2837 = ORIENTED_EDGE ( 'NONE', *, *, #7165, .T. ) ;
#2838 = PLANE ( 'NONE',  #2747 ) ;
#2839 = ORIENTED_EDGE ( 'NONE', *, *, #8183, .F. ) ;
#2840 = ORIENTED_EDGE ( 'NONE', *, *, #239, .F. ) ;
#2841 = VECTOR ( 'NONE', #10131, 1000.000000000000000 ) ;
#2842 = CARTESIAN_POINT ( 'NONE',  ( -116.5607085079957130, 236.6104925571506783, 9.460802029985586576E-16 ) ) ;
#2843 =( BOUNDED_CURVE ( )  B_SPLINE_CURVE ( 3, ( #10020, #2746, #4550, #2961 ),
 .UNSPECIFIED., .F., .F. ) 
 B_SPLINE_CURVE_WITH_KNOTS ( ( 4, 4 ),
 ( 5.245636577995398397, 5.314071712302153472 ),
 .UNSPECIFIED. ) 
 CURVE ( )  GEOMETRIC_REPRESENTATION_ITEM ( )  RATIONAL_B_SPLINE_CURVE ( ( 1.000000000000000000, 0.9996097574442918132, 0.9996097574442918132, 1.000000000000000000 ) ) 
 REPRESENTATION_ITEM ( '' )  );
#2844 = ORIENTED_EDGE ( 'NONE', *, *, #7010, .F. ) ;
#2845 = EDGE_CURVE ( 'NONE', #5058, #6361, #7654, .T. ) ;
#2846 = ORIENTED_EDGE ( 'NONE', *, *, #7542, .F. ) ;
#2847 = CARTESIAN_POINT ( 'NONE',  ( -30.29350689640809335, 120.5696653505793705, -24.00000000000000711 ) ) ;
#2848 = CYLINDRICAL_SURFACE ( 'NONE', #711, 5.000000000000000000 ) ;
#2849 = DIRECTION ( 'NONE',  ( 0.000000000000000000, 1.000000000000000000, 1.224646799147353207E-16 ) ) ;
#2850 = DIRECTION ( 'NONE',  ( 0.000000000000000000, -0.9374252720097652203, 0.3481865296036273372 ) ) ;
#2851 = DIRECTION ( 'NONE',  ( 0.000000000000000000, 0.000000000000000000, -1.000000000000000000 ) ) ;
#2852 = VECTOR ( 'NONE', #4176, 1000.000000000000000 ) ;
#2853 = DIRECTION ( 'NONE',  ( 1.000000000000000000, 0.000000000000000000, 0.000000000000000000 ) ) ;
#2854 = ORIENTED_EDGE ( 'NONE', *, *, #1220, .F. ) ;
#2855 = AXIS2_PLACEMENT_3D ( 'NONE', #4218, #6703, #6546 ) ;
#2856 = ORIENTED_EDGE ( 'NONE', *, *, #8978, .T. ) ;
#2857 = CARTESIAN_POINT ( 'NONE',  ( -23.64290342185649152, -133.6308916829187297, -50.00000000000002132 ) ) ;
#2858 = EDGE_LOOP ( 'NONE', ( #4561, #6727, #4172 ) ) ;
#2859 = EDGE_CURVE ( 'NONE', #979, #6462, #1351, .T. ) ;
#2860 = DIRECTION ( 'NONE',  ( -0.000000000000000000, -0.000000000000000000, 1.000000000000000000 ) ) ;
#2861 = CIRCLE ( 'NONE', #10326, 3.999999999999989786 ) ;
#2862 = CYLINDRICAL_SURFACE ( 'NONE', #8176, 2.000000000000001776 ) ;
#2863 = PLANE ( 'NONE',  #5875 ) ;
#2864 = ORIENTED_EDGE ( 'NONE', *, *, #3131, .T. ) ;
#2865 = ORIENTED_EDGE ( 'NONE', *, *, #10056, .T. ) ;
#2866 = CIRCLE ( 'NONE', #9658, 4.025000000000000355 ) ;
#2867 = EDGE_LOOP ( 'NONE', ( #709, #4008, #439 ) ) ;
#2868 = ORIENTED_EDGE ( 'NONE', *, *, #1888, .T. ) ;
#2869 = EDGE_CURVE ( 'NONE', #5823, #719, #2689, .T. ) ;
#2870 = DIRECTION ( 'NONE',  ( 0.000000000000000000, 1.000000000000000000, -0.000000000000000000 ) ) ;
#2871 = LINE ( 'NONE', #7699, #8487 ) ;
#2872 = EDGE_CURVE ( 'NONE', #6085, #6072, #6861, .T. ) ;
#2873 = EDGE_CURVE ( 'NONE', #3604, #1439, #7812, .T. ) ;
#2874 = CARTESIAN_POINT ( 'NONE',  ( -7.293506896408097795, -3.651280424770854409E-15, 24.99999999999998579 ) ) ;
#2875 = CARTESIAN_POINT ( 'NONE',  ( -16.29350689640809691, -8.660287962196477451, 0.000000000000000000 ) ) ;
#2876 = LINE ( 'NONE', #9082, #8908 ) ;
#2877 = ORIENTED_EDGE ( 'NONE', *, *, #5082, .F. ) ;
#2878 = DIRECTION ( 'NONE',  ( 0.000000000000000000, -0.9961946980917457672, 0.08715574274765484908 ) ) ;
#2879 = FACE_OUTER_BOUND ( 'NONE', #7608, .T. ) ;
#2880 = ADVANCED_FACE ( 'NONE', ( #2879 ), #9196, .F. ) ;
#2881 = ORIENTED_EDGE ( 'NONE', *, *, #8505, .F. ) ;
#2882 = EDGE_CURVE ( 'NONE', #6578, #8917, #9644, .T. ) ;
#2883 = EDGE_CURVE ( 'NONE', #6933, #10322, #2520, .T. ) ;
#2884 = DIRECTION ( 'NONE',  ( 0.000000000000000000, 0.000000000000000000, -1.000000000000000000 ) ) ;
#2885 = CARTESIAN_POINT ( 'NONE',  ( -16.29350689640809691, 37.08684478514406635, 0.000000000000000000 ) ) ;
#2886 = CARTESIAN_POINT ( 'NONE',  ( -8.000000000000000000, 0.000000000000000000, 0.000000000000000000 ) ) ;
#2887 = DIRECTION ( 'NONE',  ( 0.000000000000000000, 0.000000000000000000, 1.000000000000000000 ) ) ;
#2888 = EDGE_LOOP ( 'NONE', ( #7498, #7920, #2573, #7580, #7284, #6178, #5569, #1943 ) ) ;
#2889 = AXIS2_PLACEMENT_3D ( 'NONE', #5445, #9542, #10284 ) ;
#2890 = LINE ( 'NONE', #2783, #7318 ) ;
#2891 = ORIENTED_EDGE ( 'NONE', *, *, #2033, .F. ) ;
#2892 = ORIENTED_EDGE ( 'NONE', *, *, #7097, .T. ) ;
#2893 = CARTESIAN_POINT ( 'NONE',  ( 73.53765631853929108, 70.39106037767955115, -30.00000000000000355 ) ) ;
#2894 = VERTEX_POINT ( 'NONE', #400 ) ;
#2895 = EDGE_CURVE ( 'NONE', #8447, #5933, #10098, .T. ) ;
#2896 = CIRCLE ( 'NONE', #5605, 4.999999999999997335 ) ;
#2897 = ORIENTED_EDGE ( 'NONE', *, *, #5173, .T. ) ;
#2898 = CARTESIAN_POINT ( 'NONE',  ( 25.15769640663936002, -117.1457019118819005, -3.513494341946486113E-15 ) ) ;
#2899 = DIRECTION ( 'NONE',  ( -0.000000000000000000, -0.000000000000000000, 1.000000000000000000 ) ) ;
#2900 = EDGE_LOOP ( 'NONE', ( #1269, #8461, #5279, #9476, #2226, #8437, #9274, #10128, #6802, #7789, #10177, #7511, #3021, #189 ) ) ;
#2901 = CARTESIAN_POINT ( 'NONE',  ( 27.15769640663936713, -135.1457019118818721, 25.15769640663938134 ) ) ;
#2902 = CARTESIAN_POINT ( 'NONE',  ( -20.29350689640809691, 140.5696653505793563, 10.98204862120179826 ) ) ;
#2903 = DIRECTION ( 'NONE',  ( 0.000000000000000000, 0.000000000000000000, 1.000000000000000000 ) ) ;
#2904 = DIRECTION ( 'NONE',  ( -0.5150380749100536004, 0.000000000000000000, 0.8571673007021125557 ) ) ;
#2905 = EDGE_CURVE ( 'NONE', #10166, #9506, #2608, .T. ) ;
#2906 = AXIS2_PLACEMENT_3D ( 'NONE', #9156, #5073, #6771 ) ;
#2907 = TOROIDAL_SURFACE ( 'NONE', #5277, 2.525240063345735475, 5.000000000000000000 ) ;
#2908 =( BOUNDED_CURVE ( )  B_SPLINE_CURVE ( 3, ( #799, #5574, #8056, #9508 ),
 .UNSPECIFIED., .F., .T. ) 
 B_SPLINE_CURVE_WITH_KNOTS ( ( 4, 4 ),
 ( 0.9691135948774318720, 1.037548729184187168 ),
 .UNSPECIFIED. ) 
 CURVE ( )  GEOMETRIC_REPRESENTATION_ITEM ( )  RATIONAL_B_SPLINE_CURVE ( ( 1.000000000000000000, 0.9996097574442918132, 0.9996097574442918132, 1.000000000000000000 ) ) 
 REPRESENTATION_ITEM ( '' )  );
#2909 = ORIENTED_EDGE ( 'NONE', *, *, #10315, .F. ) ;
#2910 = CARTESIAN_POINT ( 'NONE',  ( -2.293506896408097795, 80.56966535057935630, 24.00000000000000711 ) ) ;
#2911 = EDGE_LOOP ( 'NONE', ( #1999, #431, #4347, #2114 ) ) ;
#2912 = LINE ( 'NONE', #10024, #9458 ) ;
#2913 = FACE_OUTER_BOUND ( 'NONE', #6832, .T. ) ;
#2914 = AXIS2_PLACEMENT_3D ( 'NONE', #5840, #237, #4308 ) ;
#2915 = AXIS2_PLACEMENT_3D ( 'NONE', #3697, #1302, #10053 ) ;
#2916 = DIRECTION ( 'NONE',  ( 0.000000000000000000, -0.000000000000000000, 1.000000000000000000 ) ) ;
#2917 = CARTESIAN_POINT ( 'NONE',  ( 77.30044127146538813, 73.68369600860394542, -25.00000000000000355 ) ) ;
#2918 = FACE_OUTER_BOUND ( 'NONE', #2931, .T. ) ;
#2919 = EDGE_LOOP ( 'NONE', ( #3689, #3554, #9337, #5592 ) ) ;
#2920 = ORIENTED_EDGE ( 'NONE', *, *, #8790, .F. ) ;
#2921 = CIRCLE ( 'NONE', #2408, 5.000000000000000888 ) ;
#2922 = AXIS2_PLACEMENT_3D ( 'NONE', #6002, #9300, #3572 ) ;
#2923 = VERTEX_POINT ( 'NONE', #2554 ) ;
#2924 = ORIENTED_EDGE ( 'NONE', *, *, #9575, .T. ) ;
#2925 = LINE ( 'NONE', #1232, #7082 ) ;
#2926 = CARTESIAN_POINT ( 'NONE',  ( 3.000000000000000000, 2.201436576420045199, 1.270999999999996355 ) ) ;
#2927 = DIRECTION ( 'NONE',  ( 0.000000000000000000, 0.000000000000000000, 1.000000000000000000 ) ) ;
#2928 = CARTESIAN_POINT ( 'NONE',  ( 23.15769640663936357, -117.1457019118819005, 27.15769640663938489 ) ) ;
#2929 = VECTOR ( 'NONE', #1808, 1000.000000000000000 ) ;
#2930 = DIRECTION ( 'NONE',  ( 0.000000000000000000, 0.000000000000000000, 1.000000000000000000 ) ) ;
#2931 = EDGE_LOOP ( 'NONE', ( #6718, #3471, #9051, #5950, #3891, #8620, #7163, #8412 ) ) ;
#2932 = CARTESIAN_POINT ( 'NONE',  ( 10.51964330236497602, 150.0000000000000000, -12.49999999999999289 ) ) ;
#2933 = EDGE_CURVE ( 'NONE', #6484, #6361, #7434, .T. ) ;
#2934 = AXIS2_PLACEMENT_3D ( 'NONE', #1159, #5973, #4339 ) ;
#2935 = DIRECTION ( 'NONE',  ( -0.7431448254773957984, 0.6691306063588565722, -0.000000000000000000 ) ) ;
#2936 = DIRECTION ( 'NONE',  ( -1.000000000000000000, -0.000000000000000000, -0.000000000000000000 ) ) ;
#2937 = DIRECTION ( 'NONE',  ( 1.000000000000000000, -0.000000000000000000, -0.000000000000000000 ) ) ;
#2938 = DIRECTION ( 'NONE',  ( -1.000000000000000000, 0.000000000000000000, 0.000000000000000000 ) ) ;
#2939 = DIRECTION ( 'NONE',  ( -1.000000000000000000, 0.000000000000000000, 0.000000000000000000 ) ) ;
#2940 = CIRCLE ( 'NONE', #9381, 4.999999999999993783 ) ;
#2941 = ORIENTED_EDGE ( 'NONE', *, *, #6494, .T. ) ;
#2942 = DIRECTION ( 'NONE',  ( -1.000000000000000000, 0.000000000000000000, 0.000000000000000000 ) ) ;
#2943 = EDGE_CURVE ( 'NONE', #3592, #2946, #8102, .T. ) ;
#2944 = EDGE_CURVE ( 'NONE', #3816, #6753, #158, .T. ) ;
#2945 = EDGE_CURVE ( 'NONE', #7279, #5671, #5627, .T. ) ;
#2946 = VERTEX_POINT ( 'NONE', #3358 ) ;
#2947 = APPLICATION_PROTOCOL_DEFINITION ( 'draft international standard', 'automotive_design', 1998, #9307 ) ;
#2948 = VERTEX_POINT ( 'NONE', #8918 ) ;
#2949 = FACE_OUTER_BOUND ( 'NONE', #6460, .T. ) ;
#2950 = ORIENTED_EDGE ( 'NONE', *, *, #744, .T. ) ;
#2951 = CIRCLE ( 'NONE', #9388, 4.999999999999997335 ) ;
#2952 = EDGE_LOOP ( 'NONE', ( #3133, #5885, #5396, #4354, #6897, #7619, #4161, #8812 ) ) ;
#2953 = DIRECTION ( 'NONE',  ( 0.000000000000000000, 1.222897680782651471E-16, 1.000000000000000000 ) ) ;
#2954 = FACE_OUTER_BOUND ( 'NONE', #9451, .T. ) ;
#2955 = CARTESIAN_POINT ( 'NONE',  ( -166.0794662972351716, 270.8019239353934040, 0.000000000000000000 ) ) ;
#2956 = ORIENTED_EDGE ( 'NONE', *, *, #7233, .T. ) ;
#2957 = CARTESIAN_POINT ( 'NONE',  ( -18.34874108452141073, -140.1746510883711778, 49.99999999999997868 ) ) ;
#2958 = MANIFOLD_SOLID_BREP ( 'CirPattern1', #4186 ) ;
#2959 = FACE_OUTER_BOUND ( 'NONE', #10440, .T. ) ;
#2960 = CARTESIAN_POINT ( 'NONE',  ( -16.29350689640809691, 88.12362273389504708, -4.729641367753004033 ) ) ;
#2961 = CARTESIAN_POINT ( 'NONE',  ( -40.99999999999999289, -3.464101615137750834, -2.000000000000019096 ) ) ;
#2962 = CARTESIAN_POINT ( 'NONE',  ( -30.29350689640809691, 140.5696653505793563, -10.98204862120179826 ) ) ;
#2963 = AXIS2_PLACEMENT_3D ( 'NONE', #3825, #3721, #534 ) ;
#2964 = EDGE_CURVE ( 'NONE', #4912, #6120, #330, .T. ) ;
#2965 = ORIENTED_EDGE ( 'NONE', *, *, #2768, .T. ) ;
#2966 = FACE_OUTER_BOUND ( 'NONE', #6308, .T. ) ;
#2967 = ORIENTED_EDGE ( 'NONE', *, *, #1066, .F. ) ;
#2968 = CARTESIAN_POINT ( 'NONE',  ( 80.08610854271792334, 54.73418909528891874, -30.00000000000000355 ) ) ;
#2969 = ORIENTED_EDGE ( 'NONE', *, *, #5288, .F. ) ;
#2970 = CARTESIAN_POINT ( 'NONE',  ( -50.00000000000002132, -135.0799149511624364, 25.93998375192767014 ) ) ;
#2971 = DIRECTION ( 'NONE',  ( 0.000000000000000000, 0.000000000000000000, -1.000000000000000000 ) ) ;
#2972 = DIRECTION ( 'NONE',  ( -0.6691306063588565722, -0.7431448254773957984, 0.000000000000000000 ) ) ;
#2973 = EDGE_LOOP ( 'NONE', ( #4647, #2422, #143, #6227 ) ) ;
#2974 = VERTEX_POINT ( 'NONE', #9780 ) ;
#2975 = PRODUCT_DEFINITION_SHAPE ( 'NONE', 'NONE',  #8524 ) ;
#2976 = EDGE_LOOP ( 'NONE', ( #1482, #1120, #9266, #1472, #5433, #9665, #2316, #2648, #674, #5990, #5400, #3667, #7202 ) ) ;
#2977 = ORIENTED_EDGE ( 'NONE', *, *, #8446, .T. ) ;
#2978 = CARTESIAN_POINT ( 'NONE',  ( -50.00000000000001421, -135.1457019118818721, -26.62179802177720944 ) ) ;
#2979 = EDGE_CURVE ( 'NONE', #3030, #7406, #3193, .T. ) ;
#2980 = DIRECTION ( 'NONE',  ( 1.000000000000000000, -0.000000000000000000, -0.000000000000000000 ) ) ;
#2981 = CARTESIAN_POINT ( 'NONE',  ( -20.29350689640809691, 140.5696653505793563, 20.00000000000002132 ) ) ;
#2982 = PLANE ( 'NONE',  #3774 ) ;
#2983 = AXIS2_PLACEMENT_3D ( 'NONE', #7778, #9371, #6986 ) ;
#2984 = DIRECTION ( 'NONE',  ( 0.000000000000000000, 0.000000000000000000, -1.000000000000000000 ) ) ;
#2985 = AXIS2_PLACEMENT_3D ( 'NONE', #297, #3520, #6749 ) ;
#2986 = EDGE_LOOP ( 'NONE', ( #4253, #1385, #9664, #1927 ) ) ;
#2987 = CARTESIAN_POINT ( 'NONE',  ( -27.15769640663940976, -133.1457019118818721, 27.15769640663938489 ) ) ;
#2988 = CIRCLE ( 'NONE', #4841, 2.000000000000001776 ) ;
#2989 = VERTEX_POINT ( 'NONE', #755 ) ;
#2990 = ORIENTED_EDGE ( 'NONE', *, *, #1128, .F. ) ;
#2991 = EDGE_LOOP ( 'NONE', ( #5729, #2029, #9643, #7770 ) ) ;
#2992 = AXIS2_PLACEMENT_3D ( 'NONE', #8735, #2421, #7201 ) ;
#2993 = ADVANCED_FACE ( 'NONE', ( #7227, #8864 ), #4926, .F. ) ;
#2994 = CARTESIAN_POINT ( 'NONE',  ( -3.173844575093148990, 105.5289575273812233, -10.90000000000000036 ) ) ;
#2995 = DIRECTION ( 'NONE',  ( 1.000000000000000000, 0.000000000000000000, -1.137729606058012035E-16 ) ) ;
#2996 = PLANE ( 'NONE',  #9928 ) ;
#2997 = AXIS2_PLACEMENT_3D ( 'NONE', #4334, #9858, #2688 ) ;
#2998 = EDGE_LOOP ( 'NONE', ( #7937, #7982, #10342, #4440 ) ) ;
#2999 = DIRECTION ( 'NONE',  ( -0.7431448254773957984, 0.6691306063588565722, -0.000000000000000000 ) ) ;
#3000 = EDGE_LOOP ( 'NONE', ( #10312, #7315 ) ) ;
#3001 = SHAPE_DEFINITION_REPRESENTATION ( #3063, #9007 ) ;
#3002 = ORIENTED_EDGE ( 'NONE', *, *, #8980, .T. ) ;
#3003 = DIRECTION ( 'NONE',  ( 0.000000000000000000, 0.000000000000000000, -1.000000000000000000 ) ) ;
#3004 = ORIENTED_EDGE ( 'NONE', *, *, #2121, .F. ) ;
#3005 = VECTOR ( 'NONE', #2507, 1000.000000000000000 ) ;
#3006 = ORIENTED_EDGE ( 'NONE', *, *, #4724, .T. ) ;
#3007 = FACE_OUTER_BOUND ( 'NONE', #2858, .T. ) ;
#3008 = EDGE_CURVE ( 'NONE', #10256, #7686, #3192, .T. ) ;
#3009 = DIRECTION ( 'NONE',  ( -1.000000000000000000, 0.000000000000000000, 0.000000000000000000 ) ) ;
#3010 = ORIENTED_EDGE ( 'NONE', *, *, #5727, .T. ) ;
#3011 = ADVANCED_FACE ( 'NONE', ( #8067 ), #7604, .F. ) ;
#3012 = CARTESIAN_POINT ( 'NONE',  ( -117.0000000000000000, -3.319229491889267081, -2.232199717805850803 ) ) ;
#3013 = CIRCLE ( 'NONE', #8931, 4.000000000000000000 ) ;
#3014 = DIRECTION ( 'NONE',  ( 0.000000000000000000, 0.000000000000000000, -1.000000000000000000 ) ) ;
#3015 = DIRECTION ( 'NONE',  ( -0.000000000000000000, 1.000000000000000000, -0.000000000000000000 ) ) ;
#3016 = FACE_OUTER_BOUND ( 'NONE', #10476, .T. ) ;
#3017 = DIRECTION ( 'NONE',  ( 0.07334937666141726209, -0.9973063064792991872, 0.000000000000000000 ) ) ;
#3018 = CIRCLE ( 'NONE', #4369, 8.703944320672444945 ) ;
#3019 = EDGE_LOOP ( 'NONE', ( #7704, #6448, #613, #6936 ) ) ;
#3020 = LINE ( 'NONE', #7895, #1802 ) ;
#3021 = ORIENTED_EDGE ( 'NONE', *, *, #1874, .T. ) ;
#3022 = DIRECTION ( 'NONE',  ( 0.000000000000000000, 0.000000000000000000, 1.000000000000000000 ) ) ;
#3023 = AXIS2_PLACEMENT_3D ( 'NONE', #480, #7583, #5927 ) ;
#3024 = EDGE_CURVE ( 'NONE', #6270, #8983, #6475, .T. ) ;
#3025 = CARTESIAN_POINT ( 'NONE',  ( -7.293506896408097795, 72.08684478514406635, 28.00000000000001066 ) ) ;
#3026 = DIRECTION ( 'NONE',  ( 0.000000000000000000, 0.000000000000000000, -1.000000000000000000 ) ) ;
#3027 = CYLINDRICAL_SURFACE ( 'NONE', #6512, 3.999999999999989786 ) ;
#3028 = CIRCLE ( 'NONE', #4380, 7.999999999999994671 ) ;
#3029 = ORIENTED_EDGE ( 'NONE', *, *, #5409, .F. ) ;
#3030 = VERTEX_POINT ( 'NONE', #5674 ) ;
#3031 = VERTEX_POINT ( 'NONE', #8117 ) ;
#3032 = AXIS2_PLACEMENT_3D ( 'NONE', #810, #7276, #16 ) ;
#3033 = ORIENTED_EDGE ( 'NONE', *, *, #3401, .F. ) ;
#3034 = CARTESIAN_POINT ( 'NONE',  ( -50.00000000000001421, -134.8487302617674857, -25.28853996896960510 ) ) ;
#3035 = DIRECTION ( 'NONE',  ( 0.000000000000000000, 0.000000000000000000, -1.000000000000000000 ) ) ;
#3036 = CARTESIAN_POINT ( 'NONE',  ( -23.15769640663937423, -115.1457019118818863, -50.00000000000002132 ) ) ;
#3037 = CARTESIAN_POINT ( 'NONE',  ( -2.293506896408097795, 145.5696653505793563, -20.00000000000000711 ) ) ;
#3038 = CARTESIAN_POINT ( 'NONE',  ( 39.99999999999998579, -135.1457019118818721, -36.00000000000002842 ) ) ;
#3039 = ORIENTED_EDGE ( 'NONE', *, *, #5529, .T. ) ;
#3040 = AXIS2_PLACEMENT_3D ( 'NONE', #230, #3454, #2661 ) ;
#3041 = DIRECTION ( 'NONE',  ( 0.000000000000000000, 0.000000000000000000, 1.000000000000000000 ) ) ;
#3042 = EDGE_CURVE ( 'NONE', #9023, #10117, #9127, .T. ) ;
#3043 = ORIENTED_EDGE ( 'NONE', *, *, #251, .T. ) ;
#3044 = DIRECTION ( 'NONE',  ( -1.396588258780021135E-16, 0.000000000000000000, 1.000000000000000000 ) ) ;
#3045 = DIRECTION ( 'NONE',  ( 0.000000000000000000, 0.000000000000000000, -1.000000000000000000 ) ) ;
#3046 = CARTESIAN_POINT ( 'NONE',  ( 4.856471286862175774, 147.5696653505793279, 25.00000000000000000 ) ) ;
#3047 = DIRECTION ( 'NONE',  ( 1.000000000000000000, -0.000000000000000000, -0.000000000000000000 ) ) ;
#3048 = ORIENTED_EDGE ( 'NONE', *, *, #7748, .T. ) ;
#3049 = FACE_OUTER_BOUND ( 'NONE', #9259, .T. ) ;
#3050 =( NAMED_UNIT ( * ) SI_UNIT ( $, .STERADIAN. ) SOLID_ANGLE_UNIT ( ) );
#3051 = ADVANCED_FACE ( 'NONE', ( #2707 ), #9177, .F. ) ;
#3052 = ORIENTED_EDGE ( 'NONE', *, *, #8775, .T. ) ;
#3053 = CARTESIAN_POINT ( 'NONE',  ( -121.7299640054770578, 230.8694527092982867, 0.000000000000000000 ) ) ;
#3054 = VERTEX_POINT ( 'NONE', #1914 ) ;
#3055 = ORIENTED_EDGE ( 'NONE', *, *, #8061, .F. ) ;
#3056 = PLANE ( 'NONE',  #9068 ) ;
#3057 = CARTESIAN_POINT ( 'NONE',  ( 27.15769640663938489, -115.1457019118818863, -25.15769640663940621 ) ) ;
#3058 = DIRECTION ( 'NONE',  ( 0.000000000000000000, 0.000000000000000000, -1.000000000000000000 ) ) ;
#3059 = DIRECTION ( 'NONE',  ( 0.000000000000000000, 0.000000000000000000, 1.000000000000000000 ) ) ;
#3060 = DIRECTION ( 'NONE',  ( -0.5000000000000051070, 1.060575238724903217E-16, -0.8660254037844355990 ) ) ;
#3061 = CARTESIAN_POINT ( 'NONE',  ( -30.29350689640809335, 0.000000000000000000, -10.98204862120179826 ) ) ;
#3062 = DIRECTION ( 'NONE',  ( -0.08084652178105139475, 0.5716988695978864055, -0.8164706010729381180 ) ) ;
#3063 = PRODUCT_DEFINITION_SHAPE ( 'NONE', 'NONE',  #3989 ) ;
#3064 = EDGE_CURVE ( 'NONE', #732, #1563, #6847, .T. ) ;
#3065 = ORIENTED_EDGE ( 'NONE', *, *, #1068, .T. ) ;
#3066 = CARTESIAN_POINT ( 'NONE',  ( -1.071796769724492338, 0.2735269159956686402, 3.990636919869545718 ) ) ;
#3067 = AXIS2_PLACEMENT_3D ( 'NONE', #7046, #2326, #9649 ) ;
#3068 = VERTEX_POINT ( 'NONE', #6740 ) ;
#3069 = CYLINDRICAL_SURFACE ( 'NONE', #6576, 1.999999999999998224 ) ;
#3070 = DIRECTION ( 'NONE',  ( -0.000000000000000000, 1.000000000000000000, -0.000000000000000000 ) ) ;
#3071 = CYLINDRICAL_SURFACE ( 'NONE', #4289, 4.024999999999997691 ) ;
#3072 = CARTESIAN_POINT ( 'NONE',  ( 42.22511195853866894, 17.84145331825995839, -25.00000000000000000 ) ) ;
#3073 = AXIS2_PLACEMENT_3D ( 'NONE', #3766, #4755, #7844 ) ;
#3074 = CYLINDRICAL_SURFACE ( 'NONE', #8374, 2.000000000000001776 ) ;
#3075 = CIRCLE ( 'NONE', #8997, 2.000000000000001776 ) ;
#3076 = ORIENTED_EDGE ( 'NONE', *, *, #10298, .T. ) ;
#3077 = MANIFOLD_SOLID_BREP ( 'Move Face4', #9619 ) ;
#3078 = ORIENTED_EDGE ( 'NONE', *, *, #6096, .F. ) ;
#3079 = EDGE_CURVE ( 'NONE', #6094, #2732, #3617, .T. ) ;
#3080 = ADVANCED_FACE ( 'NONE', ( #3510 ), #284, .T. ) ;
#3081 = EDGE_CURVE ( 'NONE', #8380, #4123, #673, .T. ) ;
#3082 = VECTOR ( 'NONE', #1634, 1000.000000000000000 ) ;
#3083 = VERTEX_POINT ( 'NONE', #7485 ) ;
#3084 = ORIENTED_EDGE ( 'NONE', *, *, #2639, .T. ) ;
#3085 = DIRECTION ( 'NONE',  ( -0.7431448254773957984, 0.6691306063588565722, -0.000000000000000000 ) ) ;
#3086 = DIRECTION ( 'NONE',  ( 1.000000000000000000, 1.112002228190260952E-16, 6.116012255046435111E-17 ) ) ;
#3087 = LINE ( 'NONE', #751, #8740 ) ;
#3088 = DIRECTION ( 'NONE',  ( -0.6691306063588565722, -0.7431448254773957984, 0.000000000000000000 ) ) ;
#3089 = CARTESIAN_POINT ( 'NONE',  ( 4.856471286862175774, 152.5696653505793279, 30.00000000000000355 ) ) ;
#3090 = VECTOR ( 'NONE', #5324, 1000.000000000000000 ) ;
#3091 = CARTESIAN_POINT ( 'NONE',  ( -2.293506896408097795, 72.08684478514408056, -28.00000000000001421 ) ) ;
#3092 = ADVANCED_FACE ( 'NONE', ( #6788 ), #166, .F. ) ;
#3093 = EDGE_LOOP ( 'NONE', ( #1645, #6402, #5095, #7331 ) ) ;
#3094 = FACE_OUTER_BOUND ( 'NONE', #2538, .T. ) ;
#3095 = CIRCLE ( 'NONE', #3428, 16.00000000000001421 ) ;
#3096 = EDGE_CURVE ( 'NONE', #9582, #1800, #2193, .T. ) ;
#3097 = DIRECTION ( 'NONE',  ( 0.000000000000000000, 0.000000000000000000, -1.000000000000000000 ) ) ;
#3098 = CYLINDRICAL_SURFACE ( 'NONE', #9731, 5.000000000000001776 ) ;
#3099 = SPHERICAL_SURFACE ( 'NONE', #9588, 2.000000000000000000 ) ;
#3100 = EDGE_LOOP ( 'NONE', ( #366, #6420, #327, #9360 ) ) ;
#3101 = FACE_OUTER_BOUND ( 'NONE', #7591, .T. ) ;
#3102 = CIRCLE ( 'NONE', #10214, 4.024999999999997691 ) ;
#3103 = SHAPE_DEFINITION_REPRESENTATION ( #10435, #3996 ) ;
#3104 = ORIENTED_EDGE ( 'NONE', *, *, #2443, .F. ) ;
#3105 = DIRECTION ( 'NONE',  ( 0.000000000000000000, 0.000000000000000000, 1.000000000000000000 ) ) ;
#3106 = ORIENTED_EDGE ( 'NONE', *, *, #4462, .T. ) ;
#3107 = EDGE_LOOP ( 'NONE', ( #3650, #6315, #5449, #2149 ) ) ;
#3108 = DIRECTION ( 'NONE',  ( -1.000000000000000000, -0.000000000000000000, -0.000000000000000000 ) ) ;
#3109 = EDGE_CURVE ( 'NONE', #4228, #9114, #338, .T. ) ;
#3110 =( NAMED_UNIT ( * ) PLANE_ANGLE_UNIT ( ) SI_UNIT ( $, .RADIAN. ) );
#3111 = DIRECTION ( 'NONE',  ( -0.7431448254773957984, 0.6691306063588565722, -0.000000000000000000 ) ) ;
#3112 = DIRECTION ( 'NONE',  ( 1.000000000000000000, 0.000000000000000000, 0.000000000000000000 ) ) ;
#3113 =( GEOMETRIC_REPRESENTATION_CONTEXT ( 3 ) GLOBAL_UNCERTAINTY_ASSIGNED_CONTEXT ( ( #9938 ) ) GLOBAL_UNIT_ASSIGNED_CONTEXT ( ( #411, #7718, #4387 ) ) REPRESENTATION_CONTEXT ( 'NONE', 'WORKASPACE' ) );
#3114 = DIRECTION ( 'NONE',  ( -1.000000000000000000, 0.000000000000000000, 0.000000000000000000 ) ) ;
#3115 = DIRECTION ( 'NONE',  ( -0.6691306063588566833, -0.7431448254773957984, 0.000000000000000000 ) ) ;
#3116 = ORIENTED_EDGE ( 'NONE', *, *, #746, .T. ) ;
#3117 = ORIENTED_EDGE ( 'NONE', *, *, #6248, .T. ) ;
#3118 = AXIS2_PLACEMENT_3D ( 'NONE', #7985, #10333, #3014 ) ;
#3119 = DIRECTION ( 'NONE',  ( -0.000000000000000000, 1.000000000000000000, -0.000000000000000000 ) ) ;
#3120 = ORIENTED_EDGE ( 'NONE', *, *, #4037, .T. ) ;
#3121 = CARTESIAN_POINT ( 'NONE',  ( 14.70649310359190309, 120.5696653505793705, -20.00000000000000711 ) ) ;
#3122 = DIRECTION ( 'NONE',  ( -1.000000000000000000, -0.000000000000000000, -0.000000000000000000 ) ) ;
#3123 = ORIENTED_EDGE ( 'NONE', *, *, #6366, .F. ) ;
#3124 = LINE ( 'NONE', #6357, #7841 ) ;
#3125 = EDGE_CURVE ( 'NONE', #4793, #2425, #7435, .T. ) ;
#3126 = DIRECTION ( 'NONE',  ( -1.000000000000000000, -0.000000000000000000, -0.000000000000000000 ) ) ;
#3127 = VECTOR ( 'NONE', #4690, 1000.000000000000000 ) ;
#3128 = CARTESIAN_POINT ( 'NONE',  ( -39.00428932080996702, 3.065011249696406370, -1.804608920635871749 ) ) ;
#3129 = ORIENTED_EDGE ( 'NONE', *, *, #3719, .F. ) ;
#3130 = ORIENTED_EDGE ( 'NONE', *, *, #8952, .F. ) ;
#3131 = EDGE_CURVE ( 'NONE', #9513, #5509, #2861, .T. ) ;
#3132 = AXIS2_PLACEMENT_3D ( 'NONE', #10347, #7161, #7905 ) ;
#3133 = ORIENTED_EDGE ( 'NONE', *, *, #3738, .F. ) ;
#3134 = CARTESIAN_POINT ( 'NONE',  ( 26.62179802177712062, -135.1457019118818721, 49.99999999999997868 ) ) ;
#3135 = AXIS2_PLACEMENT_3D ( 'NONE', #1575, #4017, #1478 ) ;
#3136 = CARTESIAN_POINT ( 'NONE',  ( -26.62179802177712773, -135.1457019118818721, -50.00000000000002132 ) ) ;
#3137 = FACE_OUTER_BOUND ( 'NONE', #9843, .T. ) ;
#3138 = EDGE_CURVE ( 'NONE', #6261, #10221, #7463, .T. ) ;
#3139 = EDGE_CURVE ( 'NONE', #7930, #7422, #1740, .T. ) ;
#3140 = EDGE_CURVE ( 'NONE', #4400, #5439, #1847, .T. ) ;
#3141 = CARTESIAN_POINT ( 'NONE',  ( -23.79350689640809335, 76.32362273389503571, -7.750000000000000000 ) ) ;
#3142 = ORIENTED_EDGE ( 'NONE', *, *, #3738, .T. ) ;
#3143 = CARTESIAN_POINT ( 'NONE',  ( -150.4057481100919915, 266.8793581191597468, 9.273919635561124944E-16 ) ) ;
#3144 = VECTOR ( 'NONE', #3534, 1000.000000000000000 ) ;
#3145 = ORIENTED_EDGE ( 'NONE', *, *, #9615, .F. ) ;
#3146 = EDGE_CURVE ( 'NONE', #1352, #6365, #8791, .T. ) ;
#3147 = DIRECTION ( 'NONE',  ( -9.776117811460147207E-16, 0.000000000000000000, 1.000000000000000000 ) ) ;
#3148 = VECTOR ( 'NONE', #8062, 1000.000000000000000 ) ;
#3149 = EDGE_CURVE ( 'NONE', #4871, #4567, #3717, .T. ) ;
#3150 = CARTESIAN_POINT ( 'NONE',  ( -160.5400390311752403, 255.6240877932848150, 0.000000000000000000 ) ) ;
#3151 = LINE ( 'NONE', #2356, #2804 ) ;
#3152 = ORIENTED_EDGE ( 'NONE', *, *, #10202, .F. ) ;
#3153 = CARTESIAN_POINT ( 'NONE',  ( 14.70649310359190309, 120.5696653505793705, -16.00000000000000711 ) ) ;
#3154 = VECTOR ( 'NONE', #1430, 1000.000000000000000 ) ;
#3155 = ORIENTED_EDGE ( 'NONE', *, *, #2550, .T. ) ;
#3156 = CIRCLE ( 'NONE', #2992, 8.000000000000000000 ) ;
#3157 = DIRECTION ( 'NONE',  ( 0.000000000000000000, 0.000000000000000000, -1.000000000000000000 ) ) ;
#3158 = ORIENTED_EDGE ( 'NONE', *, *, #2304, .F. ) ;
#3159 = EDGE_LOOP ( 'NONE', ( #8397, #7795, #2291, #6654 ) ) ;
#3160 = CIRCLE ( 'NONE', #7070, 8.703944320672444945 ) ;
#3161 = MANIFOLD_SOLID_BREP ( 'Cut-Extrude10', #8758 ) ;
#3162 = DIRECTION ( 'NONE',  ( 0.7525569905852184105, 0.6585271261848820723, 0.000000000000000000 ) ) ;
#3163 = LINE ( 'NONE', #4748, #606 ) ;
#3164 = EDGE_LOOP ( 'NONE', ( #8959, #7461, #115, #1551 ) ) ;
#3165 = SPHERICAL_SURFACE ( 'NONE', #3573, 2.000000000000000000 ) ;
#3166 = CARTESIAN_POINT ( 'NONE',  ( -155.4728935706336301, 261.2517229562222951, 0.000000000000000000 ) ) ;
#3167 = EDGE_CURVE ( 'NONE', #8341, #5589, #9757, .T. ) ;
#3168 = ORIENTED_EDGE ( 'NONE', *, *, #2125, .T. ) ;
#3169 = CIRCLE ( 'NONE', #4692, 3.999999999999989786 ) ;
#3170 = LINE ( 'NONE', #7155, #7907 ) ;
#3171 = AXIS2_PLACEMENT_3D ( 'NONE', #4196, #5035, #4978 ) ;
#3172 = EDGE_LOOP ( 'NONE', ( #7911, #8752, #2488, #3981 ) ) ;
#3173 = DIRECTION ( 'NONE',  ( -0.000000000000000000, 1.000000000000000000, -0.000000000000000000 ) ) ;
#3174 = CARTESIAN_POINT ( 'NONE',  ( 27.15769640663938489, -115.1457019118818863, -27.15769640663940976 ) ) ;
#3175 = ORIENTED_EDGE ( 'NONE', *, *, #6434, .F. ) ;
#3176 = FACE_OUTER_BOUND ( 'NONE', #9339, .T. ) ;
#3177 = CARTESIAN_POINT ( 'NONE',  ( 0.000000000000000000, 5.939536975864662969E-16, -4.700000000000000178 ) ) ;
#3178 = VECTOR ( 'NONE', #9822, 1000.000000000000000 ) ;
#3179 = CARTESIAN_POINT ( 'NONE',  ( -153.9940972124336156, 259.9202087346060921, 0.000000000000000000 ) ) ;
#3180 = VERTEX_POINT ( 'NONE', #2431 ) ;
#3181 = ORIENTED_EDGE ( 'NONE', *, *, #6146, .T. ) ;
#3182 = EDGE_CURVE ( 'NONE', #4123, #5926, #5236, .T. ) ;
#3183 = CIRCLE ( 'NONE', #1506, 3.999999999999989786 ) ;
#3184 = EDGE_LOOP ( 'NONE', ( #7189, #4392, #7724, #2651 ) ) ;
#3185 = CARTESIAN_POINT ( 'NONE',  ( -23.15769640663939199, -115.1457019118818863, -27.15769640663944173 ) ) ;
#3186 = CARTESIAN_POINT ( 'NONE',  ( -2.293506896408101348, 147.5696653505793279, 25.00000000000000000 ) ) ;
#3187 = ORIENTED_EDGE ( 'NONE', *, *, #2933, .F. ) ;
#3188 = CARTESIAN_POINT ( 'NONE',  ( -25.15769640663940976, -115.1457019118818863, -1.756747170973246291E-14 ) ) ;
#3189 = DIRECTION ( 'NONE',  ( 0.000000000000000000, -0.5000000000000011102, -0.8660254037844379305 ) ) ;
#3190 = CIRCLE ( 'NONE', #1837, 7.999999999999991118 ) ;
#3191 = EDGE_LOOP ( 'NONE', ( #3211, #1361 ) ) ;
#3192 = LINE ( 'NONE', #9672, #7264 ) ;
#3193 = CIRCLE ( 'NONE', #3544, 7.728925574020642841 ) ;
#3194 = EDGE_CURVE ( 'NONE', #5730, #5162, #945, .T. ) ;
#3195 = ADVANCED_FACE ( 'NONE', ( #5707 ), #8950, .T. ) ;
#3196 = EDGE_LOOP ( 'NONE', ( #9370, #5836, #6636, #8156, #7720 ) ) ;
#3197 = DIRECTION ( 'NONE',  ( -0.000000000000000000, 1.000000000000000000, -0.000000000000000000 ) ) ;
#3198 = VECTOR ( 'NONE', #9157, 1000.000000000000000 ) ;
#3199 = CARTESIAN_POINT ( 'NONE',  ( -16.29350689640809691, 105.5289575273812233, 7.750000000000000000 ) ) ;
#3200 = LINE ( 'NONE', #5737, #6538 ) ;
#3201 = ORIENTED_EDGE ( 'NONE', *, *, #516, .T. ) ;
#3202 = FACE_OUTER_BOUND ( 'NONE', #6399, .T. ) ;
#3203 = PRODUCT_DEFINITION ( 'UNKNOWN', '', #7860, #5677 ) ;
#3204 = EDGE_CURVE ( 'NONE', #3877, #4343, #9651, .T. ) ;
#3206 = EDGE_CURVE ( 'NONE', #7078, #3286, #5572, .T. ) ;
#3205 = ORIENTED_EDGE ( 'NONE', *, *, #387, .F. ) ;
#3207 = EDGE_CURVE ( 'NONE', #8168, #8465, #3386, .T. ) ;
#3208 = CYLINDRICAL_SURFACE ( 'NONE', #9807, 3.999999999999993339 ) ;
#3209 = AXIS2_PLACEMENT_3D ( 'NONE', #4745, #9538, #6184 ) ;
#3210 = ORIENTED_EDGE ( 'NONE', *, *, #6310, .F. ) ;
#3211 = ORIENTED_EDGE ( 'NONE', *, *, #7068, .F. ) ;
#3212 = LINE ( 'NONE', #40, #2148 ) ;
#3213 = DIRECTION ( 'NONE',  ( 0.000000000000000000, 0.000000000000000000, -1.000000000000000000 ) ) ;
#3214 = DIRECTION ( 'NONE',  ( 1.000000000000000000, 0.000000000000000000, 0.000000000000000000 ) ) ;
#3215 = FACE_OUTER_BOUND ( 'NONE', #9314, .T. ) ;
#3216 = DIRECTION ( 'NONE',  ( 0.000000000000000000, 0.000000000000000000, 1.000000000000000000 ) ) ;
#3217 = EDGE_LOOP ( 'NONE', ( #9090, #1853, #7877, #9505 ) ) ;
#3218 = EDGE_CURVE ( 'NONE', #9452, #7162, #6881, .T. ) ;
#3219 = DIRECTION ( 'NONE',  ( 0.000000000000000000, -1.000000000000000000, 0.000000000000000000 ) ) ;
#3220 = EDGE_LOOP ( 'NONE', ( #7142, #2279, #8423, #6831 ) ) ;
#3221 = DIRECTION ( 'NONE',  ( -0.7431448254773957984, 0.6691306063588565722, -0.000000000000000000 ) ) ;
#3222 = CARTESIAN_POINT ( 'NONE',  ( -40.00000000000001421, -145.1457019118819005, -40.00000000000002132 ) ) ;
#3223 = DIRECTION ( 'NONE',  ( -0.000000000000000000, -0.000000000000000000, 1.000000000000000000 ) ) ;
#3224 = LINE ( 'NONE', #7999, #9195 ) ;
#3225 = EDGE_CURVE ( 'NONE', #3083, #1282, #10064, .T. ) ;
#3226 = CARTESIAN_POINT ( 'NONE',  ( -47.94539818030328604, 155.5289575273811522, 4.000000000000000000 ) ) ;
#3227 = CARTESIAN_POINT ( 'NONE',  ( -16.29350689640809691, -115.1457019118818863, 30.31717237747080773 ) ) ;
#3228 = ORIENTED_EDGE ( 'NONE', *, *, #8889, .F. ) ;
#3229 = EDGE_LOOP ( 'NONE', ( #9255, #10422, #1280, #2204 ) ) ;
#3230 = CIRCLE ( 'NONE', #9153, 2.000000000000001776 ) ;
#3231 = ORIENTED_EDGE ( 'NONE', *, *, #8582, .F. ) ;
#3232 = ORIENTED_EDGE ( 'NONE', *, *, #2264, .T. ) ;
#3233 = CARTESIAN_POINT ( 'NONE',  ( -16.29350689640809691, 65.65569765742554864, -7.499999999999996447 ) ) ;
#3234 =( LENGTH_UNIT ( ) NAMED_UNIT ( * ) SI_UNIT ( .MILLI., .METRE. ) );
#3235 = VECTOR ( 'NONE', #3947, 1000.000000000000000 ) ;
#3236 = VECTOR ( 'NONE', #4886, 1000.000000000000000 ) ;
#3237 = CYLINDRICAL_SURFACE ( 'NONE', #2581, 4.000000000000000000 ) ;
#3238 = ORIENTED_EDGE ( 'NONE', *, *, #8687, .T. ) ;
#3239 = CARTESIAN_POINT ( 'NONE',  ( -7.293506896408098683, 126.8146633489777599, -25.00000000000000355 ) ) ;
#3240 = ORIENTED_EDGE ( 'NONE', *, *, #8119, .F. ) ;
#3241 = DIRECTION ( 'NONE',  ( -1.000000000000000000, -0.000000000000000000, -0.000000000000000000 ) ) ;
#3242 = AXIS2_PLACEMENT_3D ( 'NONE', #2428, #888, #5757 ) ;
#3243 = CONICAL_SURFACE ( 'NONE', #6635, 4.000000000000003553, 1.029744258676655200 ) ;
#3244 = ORIENTED_EDGE ( 'NONE', *, *, #5409, .T. ) ;
#3245 = ORIENTED_EDGE ( 'NONE', *, *, #3656, .T. ) ;
#3246 = DIRECTION ( 'NONE',  ( -1.387778780781445676E-16, 0.000000000000000000, 1.000000000000000000 ) ) ;
#3247 = DIRECTION ( 'NONE',  ( -0.6691306063588566833, -0.7431448254773957984, 0.000000000000000000 ) ) ;
#3248 = CIRCLE ( 'NONE', #9348, 59.51479730733485951 ) ;
#3249 = CIRCLE ( 'NONE', #1899, 4.729641367753004033 ) ;
#3250 = LINE ( 'NONE', #3366, #2620 ) ;
#3251 = EDGE_CURVE ( 'NONE', #4567, #10220, #5179, .T. ) ;
#3252 = FACE_OUTER_BOUND ( 'NONE', #2236, .T. ) ;
#3253 = ORIENTED_EDGE ( 'NONE', *, *, #5977, .T. ) ;
#3254 = DIRECTION ( 'NONE',  ( -0.000000000000000000, 1.000000000000000000, -0.000000000000000000 ) ) ;
#3255 = SHAPE_DEFINITION_REPRESENTATION ( #2218, #6561 ) ;
#3256 = ORIENTED_EDGE ( 'NONE', *, *, #5144, .F. ) ;
#3257 = TOROIDAL_SURFACE ( 'NONE', #9703, 12.02085523418795177, 4.295524112943378547 ) ;
#3258 = DIRECTION ( 'NONE',  ( -0.000000000000000000, 1.000000000000000000, -0.000000000000000000 ) ) ;
#3259 = B_SPLINE_CURVE_WITH_KNOTS ( 'NONE', 3,
 ( #3136, #9668, #9620, #8808, #1549, #4772, #6998, #2857, #2010, #1217 ),
 .UNSPECIFIED., .F., .F.,
 ( 4, 2, 2, 2, 4 ),
 ( 0.000000000000000000, 0.001023740819106960624, 0.002047481638213921248, 0.003071222457320881873, 0.004094963276427842497 ),
 .UNSPECIFIED. ) ;
#3260 = AXIS2_PLACEMENT_3D ( 'NONE', #8498, #299, #6697 ) ;
#3261 = VERTEX_POINT ( 'NONE', #6133 ) ;
#3262 = EDGE_LOOP ( 'NONE', ( #6618, #5581 ) ) ;
#3263 = CYLINDRICAL_SURFACE ( 'NONE', #8072, 7.525240063345735919 ) ;
#3264 = PLANE ( 'NONE',  #4794 ) ;
#3265 = EDGE_CURVE ( 'NONE', #125, #10166, #4557, .T. ) ;
#3266 = EDGE_CURVE ( 'NONE', #2723, #2339, #2792, .T. ) ;
#3267 = DIRECTION ( 'NONE',  ( -1.000000000000000000, -0.000000000000000000, -0.000000000000000000 ) ) ;
#3268 = CIRCLE ( 'NONE', #3951, 4.999999999999993783 ) ;
#3269 = EDGE_CURVE ( 'NONE', #3083, #9462, #2742, .T. ) ;
#3270 = DIRECTION ( 'NONE',  ( 0.000000000000000000, 1.000000000000000000, 1.460512169908342690E-16 ) ) ;
#3271 = FACE_OUTER_BOUND ( 'NONE', #4514, .T. ) ;
#3272 = EDGE_LOOP ( 'NONE', ( #4539, #2892, #3576, #2047 ) ) ;
#3273 = FACE_OUTER_BOUND ( 'NONE', #4143, .T. ) ;
#3274 = AXIS2_PLACEMENT_3D ( 'NONE', #10018, #5180, #7626 ) ;
#3275 = ORIENTED_EDGE ( 'NONE', *, *, #9064, .F. ) ;
#3276 = CARTESIAN_POINT ( 'NONE',  ( 0.000000000000000000, -145.1457019118819005, -50.00000000000002132 ) ) ;
#3277 = CARTESIAN_POINT ( 'NONE',  ( -30.29350689640809335, 120.5696653505793705, -20.00000000000000711 ) ) ;
#3278 = VECTOR ( 'NONE', #10445, 1000.000000000000000 ) ;
#3279 = DIRECTION ( 'NONE',  ( -0.7431448254773957984, 0.6691306063588565722, -0.000000000000000000 ) ) ;
#3280 = DIRECTION ( 'NONE',  ( -1.000000000000000000, 0.000000000000000000, 1.734723475976805615E-16 ) ) ;
#3281 = EDGE_CURVE ( 'NONE', #5030, #7304, #6592, .T. ) ;
#3282 = CARTESIAN_POINT ( 'NONE',  ( -38.19229777560033057, -43.28483205141633761, 12.50000000000000000 ) ) ;
#3283 = ORIENTED_EDGE ( 'NONE', *, *, #5473, .T. ) ;
#3284 = AXIS2_PLACEMENT_3D ( 'NONE', #456, #6922, #10157 ) ;
#3285 = ORIENTED_EDGE ( 'NONE', *, *, #871, .T. ) ;
#3286 = VERTEX_POINT ( 'NONE', #10121 ) ;
#3287 = ORIENTED_EDGE ( 'NONE', *, *, #3125, .F. ) ;
#3288 = EDGE_LOOP ( 'NONE', ( #4401, #5969, #4608, #8237 ) ) ;
#3289 = LINE ( 'NONE', #2492, #316 ) ;
#3290 = FACE_OUTER_BOUND ( 'NONE', #9902, .T. ) ;
#3291 = LINE ( 'NONE', #9929, #4775 ) ;
#3292 = DIRECTION ( 'NONE',  ( -0.000000000000000000, -1.000000000000000000, -0.000000000000000000 ) ) ;
#3293 = ORIENTED_EDGE ( 'NONE', *, *, #5347, .F. ) ;
#3294 = DIRECTION ( 'NONE',  ( 6.106226635438360972E-16, -1.000000000000000000, 0.000000000000000000 ) ) ;
#3295 = ORIENTED_EDGE ( 'NONE', *, *, #5202, .T. ) ;
#3296 =( NAMED_UNIT ( * ) SI_UNIT ( $, .STERADIAN. ) SOLID_ANGLE_UNIT ( ) );
#3297 = AXIS2_PLACEMENT_3D ( 'NONE', #1850, #2482, #9920 ) ;
#3298 = EDGE_CURVE ( 'NONE', #415, #6001, #7676, .T. ) ;
#3299 = ORIENTED_EDGE ( 'NONE', *, *, #8980, .F. ) ;
#3300 = AXIS2_PLACEMENT_3D ( 'NONE', #9497, #9707, #4809 ) ;
#3301 = DIRECTION ( 'NONE',  ( 0.000000000000000000, 0.000000000000000000, 1.000000000000000000 ) ) ;
#3302 = CARTESIAN_POINT ( 'NONE',  ( 26.00000000000000355, 2.994873747314852478E-16, -2.445500000000000007 ) ) ;
#3303 = DIRECTION ( 'NONE',  ( 0.000000000000000000, 0.000000000000000000, 1.000000000000000000 ) ) ;
#3304 = CARTESIAN_POINT ( 'NONE',  ( -2.293506896408097795, 152.5696653505793279, 30.00000000000000355 ) ) ;
#3305 = CARTESIAN_POINT ( 'NONE',  ( 10.26554134690924691, 64.37996872128307757, 7.749999999999998224 ) ) ;
#3306 = DIRECTION ( 'NONE',  ( 1.000000000000000000, 0.000000000000000000, 0.000000000000000000 ) ) ;
#3307 = ORIENTED_EDGE ( 'NONE', *, *, #5332, .T. ) ;
#3308 = DIRECTION ( 'NONE',  ( -0.000000000000000000, 1.000000000000000000, -0.000000000000000000 ) ) ;
#3309 = CONTEXT_DEPENDENT_SHAPE_REPRESENTATION ( #3626, #3324 ) ;
#3310 = ORIENTED_EDGE ( 'NONE', *, *, #7153, .T. ) ;
#3311 = CIRCLE ( 'NONE', #1794, 1.999999999999998224 ) ;
#3312 = CARTESIAN_POINT ( 'NONE',  ( -16.29350689640809691, -8.660287962196477451, 6.499999999999964473 ) ) ;
#3313 = EDGE_CURVE ( 'NONE', #1057, #7120, #9322, .T. ) ;
#3314 = EDGE_LOOP ( 'NONE', ( #2465, #74, #9401, #6210 ) ) ;
#3315 = CONICAL_SURFACE ( 'NONE', #9062, 4.025000000000000355, 0.7853981633975870569 ) ;
#3316 = EDGE_LOOP ( 'NONE', ( #339, #4105, #5227, #8693 ) ) ;
#3317 = DIRECTION ( 'NONE',  ( 0.000000000000000000, -1.000000000000000000, -1.222897680782651471E-16 ) ) ;
#3318 = MANIFOLD_SOLID_BREP ( 'Chamfer1', #307 ) ;
#3319 = CARTESIAN_POINT ( 'NONE',  ( -18.34874108452141783, -140.1746510883711778, -7.212905963064413228 ) ) ;
#3320 = DIRECTION ( 'NONE',  ( 0.000000000000000000, 0.000000000000000000, 1.000000000000000000 ) ) ;
#3321 = CIRCLE ( 'NONE', #953, 5.000000000000004441 ) ;
#3322 = CARTESIAN_POINT ( 'NONE',  ( -26.62179802177716326, -135.1457019118818721, 49.99999999999997868 ) ) ;
#3323 = CARTESIAN_POINT ( 'NONE',  ( -47.94539818030330025, 150.5696653505793563, 0.000000000000000000 ) ) ;
#3324 = PRODUCT_DEFINITION_SHAPE ( 'NONE', 'NONE',  #10485 ) ;
#3325 = AXIS2_PLACEMENT_3D ( 'NONE', #10406, #7175, #6160 ) ;
#3326 = VERTEX_POINT ( 'NONE', #2106 ) ;
#3327 = DIRECTION ( 'NONE',  ( 0.000000000000000000, -0.9374252720097653313, -0.3481865296036273372 ) ) ;
#3328 = EDGE_CURVE ( 'NONE', #6928, #125, #6421, .T. ) ;
#3329 = CONICAL_SURFACE ( 'NONE', #4520, 4.025000000000000355, 0.7853981633977258348 ) ;
#3330 = EDGE_CURVE ( 'NONE', #3785, #7273, #2866, .T. ) ;
#3331 = ADVANCED_FACE ( 'NONE', ( #7517 ), #9972, .F. ) ;
#3332 = ORIENTED_EDGE ( 'NONE', *, *, #8736, .T. ) ;
#3333 = DIRECTION ( 'NONE',  ( -1.000000000000000000, -0.000000000000000000, -0.000000000000000000 ) ) ;
#3334 = CARTESIAN_POINT ( 'NONE',  ( -2.293506896408097795, 120.5696653505793705, -20.00000000000000711 ) ) ;
#3335 = AXIS2_PLACEMENT_3D ( 'NONE', #3451, #2658, #9880 ) ;
#3336 = DIRECTION ( 'NONE',  ( 0.000000000000000000, 0.000000000000000000, 1.000000000000000000 ) ) ;
#3337 = AXIS2_PLACEMENT_3D ( 'NONE', #1882, #10102, #9957 ) ;
#3338 = DIRECTION ( 'NONE',  ( -1.000000000000000000, -0.000000000000000000, -0.000000000000000000 ) ) ;
#3339 = LINE ( 'NONE', #7465, #71 ) ;
#3340 = CARTESIAN_POINT ( 'NONE',  ( 53.40242741783141156, 52.77167129626698028, -25.00000000000000355 ) ) ;
#3341 = VERTEX_POINT ( 'NONE', #322 ) ;
#3342 = AXIS2_PLACEMENT_3D ( 'NONE', #2453, #8017, #814 ) ;
#3343 = ORIENTED_EDGE ( 'NONE', *, *, #856, .F. ) ;
#3344 = ORIENTED_EDGE ( 'NONE', *, *, #2751, .T. ) ;
#3345 = AXIS2_PLACEMENT_3D ( 'NONE', #175, #120, #3354 ) ;
#3346 = ADVANCED_FACE ( 'NONE', ( #3548 ), #9215, .F. ) ;
#3347 = ORIENTED_EDGE ( 'NONE', *, *, #1454, .T. ) ;
#3348 = EDGE_CURVE ( 'NONE', #6390, #8880, #725, .T. ) ;
#3349 = CARTESIAN_POINT ( 'NONE',  ( -56.36957570605427037, 137.0132282531173473, -4.025000000000000355 ) ) ;
#3350 = CARTESIAN_POINT ( 'NONE',  ( -48.00000000000002132, -135.1457019118818721, -23.15769640663945594 ) ) ;
#3351 = AXIS2_PLACEMENT_3D ( 'NONE', #6743, #7438, #8334 ) ;
#3352 = APPLICATION_CONTEXT ( 'automotive_design' ) ;
#3353 = DIRECTION ( 'NONE',  ( -1.000000000000000000, 0.000000000000000000, 0.000000000000000000 ) ) ;
#3354 = DIRECTION ( 'NONE',  ( 0.000000000000000000, 0.000000000000000000, 1.000000000000000000 ) ) ;
#3355 = VERTEX_POINT ( 'NONE', #6289 ) ;
#3356 = DIRECTION ( 'NONE',  ( 0.000000000000000000, 0.000000000000000000, 1.000000000000000000 ) ) ;
#3357 = ORIENTED_EDGE ( 'NONE', *, *, #4109, .F. ) ;
#3358 = CARTESIAN_POINT ( 'NONE',  ( -30.29350689640809335, 80.56966535057935630, 16.00000000000000711 ) ) ;
#3359 = VERTEX_POINT ( 'NONE', #2957 ) ;
#3360 = UNCERTAINTY_MEASURE_WITH_UNIT (LENGTH_MEASURE( 1.000000000000000082E-05 ), #7398, 'distance_accuracy_value', 'NONE');
#3361 = ORIENTED_EDGE ( 'NONE', *, *, #6996, .T. ) ;
#3362 = CARTESIAN_POINT ( 'NONE',  ( -16.29350689640809691, 88.12362273389504708, 0.000000000000000000 ) ) ;
#3363 = PLANE ( 'NONE',  #2469 ) ;
#3364 = CARTESIAN_POINT ( 'NONE',  ( 53.40242741783141156, 52.77167129626698028, 30.00000000000000355 ) ) ;
#3365 = AXIS2_PLACEMENT_3D ( 'NONE', #2599, #5982, #3715 ) ;
#3366 = CARTESIAN_POINT ( 'NONE',  ( 2.108096605167896559E-14, -133.1457019118818721, -25.15769640663943107 ) ) ;
#3367 = EDGE_CURVE ( 'NONE', #8668, #4826, #1855, .T. ) ;
#3368 = CARTESIAN_POINT ( 'NONE',  ( 37.65645052921861691, -135.1457019118819289, -27.03605397352983175 ) ) ;
#3369 = EDGE_LOOP ( 'NONE', ( #6942, #1272, #1590, #5013 ) ) ;
#3370 = DIRECTION ( 'NONE',  ( 0.000000000000000000, -1.000000000000000000, 1.329743448921561232E-15 ) ) ;
#3371 = ORIENTED_EDGE ( 'NONE', *, *, #9788, .F. ) ;
#3372 = DIRECTION ( 'NONE',  ( -1.000000000000000000, -0.000000000000000000, -0.000000000000000000 ) ) ;
#3373 = ORIENTED_EDGE ( 'NONE', *, *, #2280, .T. ) ;
#3374 = VECTOR ( 'NONE', #553, 1000.000000000000000 ) ;
#3375 = DIRECTION ( 'NONE',  ( 0.000000000000000000, -1.000000000000000000, 0.000000000000000000 ) ) ;
#3376 = DIRECTION ( 'NONE',  ( 0.000000000000000000, -0.4999999999999985567, 0.8660254037844394848 ) ) ;
#3377 = PLANE ( 'NONE',  #1278 ) ;
#3378 = PLANE ( 'NONE',  #6960 ) ;
#3379 = LINE ( 'NONE', #1038, #1051 ) ;
#3380=STYLED_ITEM('',(#10511),#3161);
#3381 = VERTEX_POINT ( 'NONE', #2366 ) ;
#3382 = DIRECTION ( 'NONE',  ( 0.000000000000000000, 0.000000000000000000, 1.000000000000000000 ) ) ;
#3383 = ORIENTED_EDGE ( 'NONE', *, *, #4237, .T. ) ;
#3384 = CARTESIAN_POINT ( 'NONE',  ( -2.293506896408097795, 120.5696653505793705, -20.00000000000000711 ) ) ;
#3385 = CARTESIAN_POINT ( 'NONE',  ( 18.34874108452142494, -140.1746510883711778, 49.99999999999997868 ) ) ;
#3386 = LINE ( 'NONE', #5816, #6414 ) ;
#3387 = CARTESIAN_POINT ( 'NONE',  ( 0.000000000000000000, -2.935248768560057009, 4.770489558936219510E-15 ) ) ;
#3388 = DIRECTION ( 'NONE',  ( -8.379529552680124346E-16, 0.000000000000000000, 1.000000000000000000 ) ) ;
#3389 = CARTESIAN_POINT ( 'NONE',  ( -8.793506896408100459, 76.32362273389503571, 7.750000000000014211 ) ) ;
#3390 = EDGE_CURVE ( 'NONE', #1816, #6696, #6345, .T. ) ;
#3391 = ORIENTED_EDGE ( 'NONE', *, *, #2219, .T. ) ;
#3392 = ORIENTED_EDGE ( 'NONE', *, *, #5271, .F. ) ;
#3393 = VERTEX_POINT ( 'NONE', #9481 ) ;
#3394 = CARTESIAN_POINT ( 'NONE',  ( -11.29350689640809158, 105.5289575273812233, -25.04213562373096380 ) ) ;
#3395 = CARTESIAN_POINT ( 'NONE',  ( -2.293506896408097795, 37.08684478514406635, 30.00000000000000355 ) ) ;
#3396 = CARTESIAN_POINT ( 'NONE',  ( -30.29350689640809335, 120.5696653505793705, 20.00000000000000711 ) ) ;
#3397 = DIRECTION ( 'NONE',  ( -1.000000000000000000, 0.000000000000000000, 0.000000000000000000 ) ) ;
#3398 = AXIS2_PLACEMENT_3D ( 'NONE', #7312, #9814, #4287 ) ;
#3399 = ADVANCED_FACE ( 'NONE', ( #7886 ), #8676, .F. ) ;
#3400 = DIRECTION ( 'NONE',  ( -1.000000000000000000, -0.000000000000000000, -0.000000000000000000 ) ) ;
#3401 = EDGE_CURVE ( 'NONE', #4076, #7523, #2364, .T. ) ;
#3402 = EDGE_CURVE ( 'NONE', #3742, #3545, #3724, .T. ) ;
#3403 = VERTEX_POINT ( 'NONE', #10332 ) ;
#3404 = CARTESIAN_POINT ( 'NONE',  ( -25.15769640663940621, -115.1457019118818863, 23.15769640663938134 ) ) ;
#3405 = ORIENTED_EDGE ( 'NONE', *, *, #10002, .T. ) ;
#3406 = CIRCLE ( 'NONE', #198, 5.000000000000007994 ) ;
#3407 = ORIENTED_EDGE ( 'NONE', *, *, #6053, .T. ) ;
#3408 = LINE ( 'NONE', #7382, #10297 ) ;
#3409 = DIRECTION ( 'NONE',  ( 0.000000000000000000, 0.000000000000000000, 1.000000000000000000 ) ) ;
#3410 = CARTESIAN_POINT ( 'NONE',  ( -2.293506896408097795, 0.000000000000000000, 10.98204862120179826 ) ) ;
#3411 = DIRECTION ( 'NONE',  ( -0.000000000000000000, -0.000000000000000000, 1.000000000000000000 ) ) ;
#3412 = CARTESIAN_POINT ( 'NONE',  ( -36.36957570605426326, 137.0132282531173473, -4.000000000000003553 ) ) ;
#3413 = VECTOR ( 'NONE', #2643, 1000.000000000000000 ) ;
#3414 = ADVANCED_FACE ( 'NONE', ( #9591 ), #5389, .T. ) ;
#3415 = ORIENTED_EDGE ( 'NONE', *, *, #6587, .F. ) ;
#3416=STYLED_ITEM('',(#10518),#10321);
#3417 = CARTESIAN_POINT ( 'NONE',  ( 42.22511195853867605, 17.84145331825995839, 30.00000000000000355 ) ) ;
#3418 = ITEM_DEFINED_TRANSFORMATION ( 'NONE', 'NONE', #4641,  #4601 ) ;
#3419 = VERTEX_POINT ( 'NONE', #5442 ) ;
#3420 = CARTESIAN_POINT ( 'NONE',  ( 5.999999999999998224, 6.123233995736766282E-16, -5.000000000000000000 ) ) ;
#3421 = ORIENTED_EDGE ( 'NONE', *, *, #4237, .F. ) ;
#3422 = CIRCLE ( 'NONE', #2745, 3.999999999999998668 ) ;
#3423 = CIRCLE ( 'NONE', #540, 2.000000000000001776 ) ;
#3424 = DIRECTION ( 'NONE',  ( 0.000000000000000000, 0.000000000000000000, 1.000000000000000000 ) ) ;
#3425 = CARTESIAN_POINT ( 'NONE',  ( 59.99999999999999289, -135.1457019118818721, -40.00000000000000000 ) ) ;
#3426 = DIRECTION ( 'NONE',  ( 0.000000000000000000, -1.000000000000000000, 0.000000000000000000 ) ) ;
#3427 = CARTESIAN_POINT ( 'NONE',  ( 99.80027788547049283, -145.1457019118819005, -24.99999999999998934 ) ) ;
#3428 = AXIS2_PLACEMENT_3D ( 'NONE', #9716, #7072, #9621 ) ;
#3429 = VECTOR ( 'NONE', #2686, 1000.000000000000000 ) ;
#3430 = ORIENTED_EDGE ( 'NONE', *, *, #3690, .F. ) ;
#3431 = DIRECTION ( 'NONE',  ( -0.000000000000000000, 1.000000000000000000, -0.000000000000000000 ) ) ;
#3432 = ADVANCED_FACE ( 'NONE', ( #7099 ), #1476, .F. ) ;
#3433 = EDGE_LOOP ( 'NONE', ( #3804, #1063, #3002, #4595 ) ) ;
#3434 = FACE_OUTER_BOUND ( 'NONE', #8159, .T. ) ;
#3435 = CARTESIAN_POINT ( 'NONE',  ( -27.15769640663939555, -133.1457019118818721, -25.15769640663944173 ) ) ;
#3436 = SURFACE_STYLE_USAGE ( .BOTH. , #8098 ) ;
#3437 = DIRECTION ( 'NONE',  ( 0.000000000000000000, 0.000000000000000000, -1.000000000000000000 ) ) ;
#3438 = DIRECTION ( 'NONE',  ( -1.000000000000000000, -0.000000000000000000, -0.000000000000000000 ) ) ;
#3439 = DIRECTION ( 'NONE',  ( 0.000000000000000000, 0.000000000000000000, 1.000000000000000000 ) ) ;
#3440 = MANIFOLD_SOLID_BREP ( 'Cut-Extrude11', #4359 ) ;
#3441 = VERTEX_POINT ( 'NONE', #3753 ) ;
#3442 = ORIENTED_EDGE ( 'NONE', *, *, #3993, .F. ) ;
#3443 = AXIS2_PLACEMENT_3D ( 'NONE', #4909, #892, #2432 ) ;
#3444 = ORIENTED_EDGE ( 'NONE', *, *, #2247, .F. ) ;
#3445 = ADVANCED_FACE ( 'NONE', ( #3963 ), #679, .T. ) ;
#3446 = DIRECTION ( 'NONE',  ( 0.000000000000000000, -1.000000000000000000, 1.431206729101514631E-16 ) ) ;
#3447 = DIRECTION ( 'NONE',  ( 0.000000000000000000, 0.000000000000000000, 1.000000000000000000 ) ) ;
#3448 = CYLINDRICAL_SURFACE ( 'NONE', #4857, 7.500000000000000000 ) ;
#3449 = CIRCLE ( 'NONE', #2436, 4.000000000000000000 ) ;
#3450 = ORIENTED_EDGE ( 'NONE', *, *, #7348, .T. ) ;
#3451 = CARTESIAN_POINT ( 'NONE',  ( -7.293506896408097795, 0.000000000000000000, 0.000000000000000000 ) ) ;
#3452 = PRODUCT_DEFINITION_FORMATION_WITH_SPECIFIED_SOURCE ( 'ANY', '', #7892, .NOT_KNOWN. ) ;
#3453 = VERTEX_POINT ( 'NONE', #10226 ) ;
#3454 = DIRECTION ( 'NONE',  ( -1.000000000000000000, 0.000000000000000000, 0.000000000000000000 ) ) ;
#3455 = AXIS2_PLACEMENT_3D ( 'NONE', #4155, #1767, #24 ) ;
#3456 = EDGE_LOOP ( 'NONE', ( #2128, #9966, #6278, #6714 ) ) ;
#3457 = UNCERTAINTY_MEASURE_WITH_UNIT (LENGTH_MEASURE( 1.000000000000000082E-05 ), #7613, 'distance_accuracy_value', 'NONE');
#3458 = ORIENTED_EDGE ( 'NONE', *, *, #1491, .T. ) ;
#3459 = EDGE_CURVE ( 'NONE', #1518, #732, #575, .T. ) ;
#3460 = DIRECTION ( 'NONE',  ( 0.000000000000000000, 1.000000000000000000, 0.000000000000000000 ) ) ;
#3461 = ADVANCED_FACE ( 'NONE', ( #8938 ), #2490, .F. ) ;
#3462 = PLANE ( 'NONE',  #2048 ) ;
#3463 = ADVANCED_FACE ( 'NONE', ( #5693 ), #8988, .F. ) ;
#3464 = LINE ( 'NONE', #2666, #8051 ) ;
#3465 = LINE ( 'NONE', #1921, #6992 ) ;
#3466 = CARTESIAN_POINT ( 'NONE',  ( -161.3589532509997468, 266.5515548974023545, 0.000000000000000000 ) ) ;
#3467 = AXIS2_PLACEMENT_3D ( 'NONE', #9867, #8152, #3439 ) ;
#3468 = ORIENTED_EDGE ( 'NONE', *, *, #10147, .T. ) ;
#3469 = CARTESIAN_POINT ( 'NONE',  ( -40.00000000000002842, -135.1457019118818721, 44.02499999999997726 ) ) ;
#3470 = CIRCLE ( 'NONE', #3818, 5.000000000000004441 ) ;
#3471 = ORIENTED_EDGE ( 'NONE', *, *, #6433, .T. ) ;
#3472 = PLANE ( 'NONE',  #3890 ) ;
#3473 = ORIENTED_EDGE ( 'NONE', *, *, #8527, .T. ) ;
#3474 = ADVANCED_FACE ( 'NONE', ( #5803, #2466, #9688, #2416, #5645 ), #4898, .T. ) ;
#3475 = AXIS2_PLACEMENT_3D ( 'NONE', #7943, #9593, #5391 ) ;
#3476 = CARTESIAN_POINT ( 'NONE',  ( 3.000000000000000000, 1.467624384280032501, 2.541999999999999371 ) ) ;
#3477 = CARTESIAN_POINT ( 'NONE',  ( 37.22759939293836595, -133.1457019118818721, 25.15769640663938134 ) ) ;
#3478 = DIRECTION ( 'NONE',  ( -0.000000000000000000, -0.000000000000000000, -1.000000000000000000 ) ) ;
#3479 = DIRECTION ( 'NONE',  ( 0.000000000000000000, -1.000000000000000000, 0.000000000000000000 ) ) ;
#3480 = CARTESIAN_POINT ( 'NONE',  ( -2.293506896408097795, 147.5696653505793279, -30.00000000000000355 ) ) ;
#3481 = DIRECTION ( 'NONE',  ( 0.000000000000000000, 0.000000000000000000, 1.000000000000000000 ) ) ;
#3482 = ORIENTED_EDGE ( 'NONE', *, *, #2473, .T. ) ;
#3483 = CIRCLE ( 'NONE', #3995, 2.000000000000001776 ) ;
#3484 = CARTESIAN_POINT ( 'NONE',  ( 3.000000000000000000, -2.935248768560057009, 4.770489558936219510E-15 ) ) ;
#3485 = ORIENTED_EDGE ( 'NONE', *, *, #2669, .F. ) ;
#3486 = CARTESIAN_POINT ( 'NONE',  ( -99.71820871057254010, 205.6674483012464520, 0.000000000000000000 ) ) ;
#3487 = CARTESIAN_POINT ( 'NONE',  ( -3.173844575093148990, 130.5696653505793847, -7.750000000000000000 ) ) ;
#3488 = AXIS2_PLACEMENT_3D ( 'NONE', #5331, #6237, #4544 ) ;
#3489 =( NAMED_UNIT ( * ) SI_UNIT ( $, .STERADIAN. ) SOLID_ANGLE_UNIT ( ) );
#3490 = CYLINDRICAL_SURFACE ( 'NONE', #3789, 5.000000000000004441 ) ;
#3491 = CARTESIAN_POINT ( 'NONE',  ( -30.29350689640809335, 88.56966535057934209, -20.00000000000001066 ) ) ;
#3492 = AXIS2_PLACEMENT_3D ( 'NONE', #7019, #2930, #703 ) ;
#3493 = FACE_OUTER_BOUND ( 'NONE', #5123, .T. ) ;
#3494 = EDGE_CURVE ( 'NONE', #6362, #10164, #5867, .T. ) ;
#3495 = EDGE_LOOP ( 'NONE', ( #10460, #8665, #7061, #4765 ) ) ;
#3496 = ORIENTED_EDGE ( 'NONE', *, *, #7879, .F. ) ;
#3497 = AXIS2_PLACEMENT_3D ( 'NONE', #7840, #2115, #4658 ) ;
#3498 = EDGE_CURVE ( 'NONE', #996, #6001, #1303, .T. ) ;
#3499 = AXIS2_PLACEMENT_3D ( 'NONE', #2370, #3017, #4800 ) ;
#3500 = ORIENTED_EDGE ( 'NONE', *, *, #4372, .T. ) ;
#3501 = FACE_OUTER_BOUND ( 'NONE', #1979, .T. ) ;
#3502 = LINE ( 'NONE', #6839, #10026 ) ;
#3503 = LINE ( 'NONE', #2702, #6141 ) ;
#3504 = CARTESIAN_POINT ( 'NONE',  ( 49.99999999999997158, -145.1457019118819005, 39.99999999999997868 ) ) ;
#3505 = VECTOR ( 'NONE', #8202, 1000.000000000000000 ) ;
#3506 = ORIENTED_EDGE ( 'NONE', *, *, #3064, .T. ) ;
#3507 = DIRECTION ( 'NONE',  ( 0.000000000000000000, -0.000000000000000000, -1.000000000000000000 ) ) ;
#3508 = VERTEX_POINT ( 'NONE', #1572 ) ;
#3509=STYLED_ITEM('',(#10497),#3440);
#3510 = FACE_OUTER_BOUND ( 'NONE', #7003, .T. ) ;
#3511 = ADVANCED_FACE ( 'NONE', ( #148 ), #8243, .F. ) ;
#3512 = VECTOR ( 'NONE', #2936, 1000.000000000000000 ) ;
#3513 = VERTEX_POINT ( 'NONE', #4221 ) ;
#3514 = DIRECTION ( 'NONE',  ( -0.000000000000000000, -0.000000000000000000, 1.000000000000000000 ) ) ;
#3515 = CARTESIAN_POINT ( 'NONE',  ( 27.15769640663937068, -135.1457019118818721, 47.99999999999997868 ) ) ;
#3516 = VECTOR ( 'NONE', #7691, 1000.000000000000000 ) ;
#3517 = FACE_OUTER_BOUND ( 'NONE', #10362, .T. ) ;
#3518 = DIRECTION ( 'NONE',  ( 0.000000000000000000, 1.000000000000000000, -0.000000000000000000 ) ) ;
#3519 = FACE_OUTER_BOUND ( 'NONE', #5635, .T. ) ;
#3520 = DIRECTION ( 'NONE',  ( -0.000000000000000000, 1.000000000000000000, -0.000000000000000000 ) ) ;
#3521 = ORIENTED_EDGE ( 'NONE', *, *, #7956, .T. ) ;
#3522 = LINE ( 'NONE', #2083, #374 ) ;
#3523 = ADVANCED_FACE ( 'NONE', ( #2522, #5748 ), #4115, .F. ) ;
#3524 = EDGE_CURVE ( 'NONE', #2357, #8114, #4355, .T. ) ;
#3525 = ORIENTED_EDGE ( 'NONE', *, *, #4374, .F. ) ;
#3526 = DIRECTION ( 'NONE',  ( 1.000000000000000000, -0.000000000000000000, -1.223202451009287022E-16 ) ) ;
#3527 = ADVANCED_FACE ( 'NONE', ( #9905 ), #8031, .F. ) ;
#3528 = ORIENTED_EDGE ( 'NONE', *, *, #4829, .T. ) ;
#3529 = VECTOR ( 'NONE', #5243, 1000.000000000000227 ) ;
#3530 =( LENGTH_UNIT ( ) NAMED_UNIT ( * ) SI_UNIT ( .MILLI., .METRE. ) );
#3531 = ORIENTED_EDGE ( 'NONE', *, *, #10340, .F. ) ;
#3532 = CARTESIAN_POINT ( 'NONE',  ( 25.15769640663938844, -117.1457019118819005, -50.00000000000002132 ) ) ;
#3533 = CARTESIAN_POINT ( 'NONE',  ( -27.85255513972543895, 64.37996872128307757, -7.749999999999996447 ) ) ;
#3534 = DIRECTION ( 'NONE',  ( -0.000000000000000000, -0.000000000000000000, -1.000000000000000000 ) ) ;
#3535 = DIRECTION ( 'NONE',  ( -0.000000000000000000, -0.000000000000000000, -1.000000000000000000 ) ) ;
#3536 = EDGE_LOOP ( 'NONE', ( #6504, #5691, #8029 ) ) ;
#3537 = DIRECTION ( 'NONE',  ( -1.000000000000000000, -0.000000000000000000, 0.000000000000000000 ) ) ;
#3538 = EDGE_CURVE ( 'NONE', #5630, #6595, #7293, .T. ) ;
#3539 = ADVANCED_FACE ( 'NONE', ( #773 ), #5593, .F. ) ;
#3540 = EDGE_CURVE ( 'NONE', #6595, #8048, #3212, .T. ) ;
#3541 = DIRECTION ( 'NONE',  ( 0.000000000000000000, 0.000000000000000000, 1.000000000000000000 ) ) ;
#3542 = ORIENTED_EDGE ( 'NONE', *, *, #9304, .F. ) ;
#3543 = FACE_OUTER_BOUND ( 'NONE', #3456, .T. ) ;
#3544 = AXIS2_PLACEMENT_3D ( 'NONE', #1704, #8014, #6422 ) ;
#3545 = VERTEX_POINT ( 'NONE', #7246 ) ;
#3546 = CARTESIAN_POINT ( 'NONE',  ( -47.94539818030328604, 70.52895752738115220, 0.000000000000000000 ) ) ;
#3547 = LINE ( 'NONE', #418, #9530 ) ;
#3548 = FACE_OUTER_BOUND ( 'NONE', #4416, .T. ) ;
#3549 = DIRECTION ( 'NONE',  ( -1.000000000000000000, 0.000000000000000000, 0.000000000000000000 ) ) ;
#3550 = FACE_OUTER_BOUND ( 'NONE', #5042, .T. ) ;
#3551 = CARTESIAN_POINT ( 'NONE',  ( -30.29350689640809335, 50.54838324668256888, -20.00000000000001776 ) ) ;
#3552 = AXIS2_PLACEMENT_3D ( 'NONE', #1865, #384, #9126 ) ;
#3553 = ADVANCED_FACE ( 'NONE', ( #6439 ), #3263, .T. ) ;
#3554 = ORIENTED_EDGE ( 'NONE', *, *, #8653, .T. ) ;
#3555 = EDGE_LOOP ( 'NONE', ( #4070, #8995, #4266 ) ) ;
#3556 = CARTESIAN_POINT ( 'NONE',  ( 0.000000000000000000, -115.1457019118818863, 23.15769640663938134 ) ) ;
#3557 = ADVANCED_FACE ( 'NONE', ( #5956 ), #9308, .T. ) ;
#3558 = DIRECTION ( 'NONE',  ( 7.848480207562752404E-17, -1.000000000000000000, -8.929448294704472850E-33 ) ) ;
#3559 = CARTESIAN_POINT ( 'NONE',  ( -50.00000000000001421, -134.0910007290637509, 24.15108826162072120 ) ) ;
#3560 = LINE ( 'NONE', #10028, #10302 ) ;
#3561 = VERTEX_POINT ( 'NONE', #6920 ) ;
#3562 = DIRECTION ( 'NONE',  ( 0.000000000000000000, 0.000000000000000000, 1.000000000000000000 ) ) ;
#3563 = ORIENTED_EDGE ( 'NONE', *, *, #9874, .F. ) ;
#3564 = ORIENTED_EDGE ( 'NONE', *, *, #10042, .T. ) ;
#3565 = DIRECTION ( 'NONE',  ( -8.194486552889013533E-17, -9.100899318238110877E-17, 1.000000000000000000 ) ) ;
#3566 = EDGE_CURVE ( 'NONE', #5617, #2069, #403, .T. ) ;
#3567 = CARTESIAN_POINT ( 'NONE',  ( -16.29350689640809691, 105.5289575273812233, 7.750000000000000000 ) ) ;
#3568 = CARTESIAN_POINT ( 'NONE',  ( 0.000000000000000000, -117.1457019118819005, 25.15769640663938134 ) ) ;
#3569 = DIRECTION ( 'NONE',  ( -0.000000000000000000, -1.000000000000000000, 0.000000000000000000 ) ) ;
#3570 = DIRECTION ( 'NONE',  ( -1.000000000000000000, 0.000000000000000000, 0.000000000000000000 ) ) ;
#3571 = ORIENTED_EDGE ( 'NONE', *, *, #1516, .T. ) ;
#3572 = DIRECTION ( 'NONE',  ( 0.000000000000000000, 0.000000000000000000, 1.000000000000000000 ) ) ;
#3573 = AXIS2_PLACEMENT_3D ( 'NONE', #2273, #1425, #10335 ) ;
#3574 = ORIENTED_EDGE ( 'NONE', *, *, #8155, .F. ) ;
#3575 = DIRECTION ( 'NONE',  ( -0.7431448254773957984, 0.6691306063588565722, -0.000000000000000000 ) ) ;
#3576 = ORIENTED_EDGE ( 'NONE', *, *, #3459, .F. ) ;
#3577 = ADVANCED_FACE ( 'NONE', ( #5164 ), #1832, .T. ) ;
#3578 = VECTOR ( 'NONE', #4263, 1000.000000000000000 ) ;
#3579 = LINE ( 'NONE', #3532, #5697 ) ;
#3580 = LINE ( 'NONE', #253, #5644 ) ;
#3581 = DIRECTION ( 'NONE',  ( -0.000000000000000000, 1.000000000000000000, -0.000000000000000000 ) ) ;
#3582 = DIRECTION ( 'NONE',  ( 0.000000000000000000, 1.000000000000000000, 0.000000000000000000 ) ) ;
#3583 = ORIENTED_EDGE ( 'NONE', *, *, #745, .T. ) ;
#3584 = CARTESIAN_POINT ( 'NONE',  ( -16.29350689640809691, -8.660287962196477451, 4.999999999999995559 ) ) ;
#3585 = ORIENTED_EDGE ( 'NONE', *, *, #7838, .F. ) ;
#3586 = CARTESIAN_POINT ( 'NONE',  ( 0.000000000000000000, 0.000000000000000000, 0.000000000000000000 ) ) ;
#3587 = VERTEX_POINT ( 'NONE', #7659 ) ;
#3588 = PRESENTATION_LAYER_ASSIGNMENT (  '', '', ( #5770 ) ) ;
#3589 = DIRECTION ( 'NONE',  ( 0.000000000000000000, 0.5000000000000012212, 0.8660254037844379305 ) ) ;
#3590 = AXIS2_PLACEMENT_3D ( 'NONE', #3610, #6144, #433 ) ;
#3591 =( BOUNDED_CURVE ( )  B_SPLINE_CURVE ( 3, ( #10457, #6268, #7125, #7272 ),
 .UNSPECIFIED., .F., .T. ) 
 B_SPLINE_CURVE_WITH_KNOTS ( ( 4, 4 ),
 ( 1.570796326794896558, 4.712388980384689674 ),
 .UNSPECIFIED. ) 
 CURVE ( )  GEOMETRIC_REPRESENTATION_ITEM ( )  RATIONAL_B_SPLINE_CURVE ( ( 1.000000000000000000, 0.3333333333333333703, 0.3333333333333333703, 1.000000000000000000 ) ) 
 REPRESENTATION_ITEM ( '' )  );
#3592 = VERTEX_POINT ( 'NONE', #7504 ) ;
#3593 = FACE_OUTER_BOUND ( 'NONE', #4251, .T. ) ;
#3594 = EDGE_CURVE ( 'NONE', #979, #3261, #6064, .T. ) ;
#3595 = DIRECTION ( 'NONE',  ( -1.000000000000000000, 0.000000000000000000, 9.101836848464095537E-17 ) ) ;
#3596 = ADVANCED_FACE ( 'NONE', ( #6707 ), #6864, .T. ) ;
#3597 = EDGE_CURVE ( 'NONE', #382, #9513, #5853, .T. ) ;
#3598 = CARTESIAN_POINT ( 'NONE',  ( 67.68113203623319407, 150.5696653505793563, -10.98204862120179826 ) ) ;
#3599 = CARTESIAN_POINT ( 'NONE',  ( 0.3000000000000016542, 6.123233995736766282E-16, -5.000000000000000000 ) ) ;
#3600 = DIRECTION ( 'NONE',  ( -0.000000000000000000, -0.000000000000000000, 1.000000000000000000 ) ) ;
#3601 = VECTOR ( 'NONE', #4649, 1000.000000000000000 ) ;
#3602 = DIRECTION ( 'NONE',  ( 1.000000000000000000, 0.000000000000000000, 0.000000000000000000 ) ) ;
#3603 = VECTOR ( 'NONE', #4067, 1000.000000000000000 ) ;
#3604 = VERTEX_POINT ( 'NONE', #6808 ) ;
#3605 = EDGE_LOOP ( 'NONE', ( #6326, #5462, #695, #8763 ) ) ;
#3606 = ADVANCED_FACE ( 'NONE', ( #2036, #252, #5263 ), #10003, .F. ) ;
#3607 = AXIS2_PLACEMENT_3D ( 'NONE', #9456, #5362, #5417 ) ;
#3608 = AXIS2_PLACEMENT_3D ( 'NONE', #4474, #451, #2030 ) ;
#3609 = CARTESIAN_POINT ( 'NONE',  ( -166.5958414309862690, 248.8984378607219980, 0.000000000000000000 ) ) ;
#3610 = CARTESIAN_POINT ( 'NONE',  ( 14.70649310359190309, 80.56966535057935630, 20.00000000000000711 ) ) ;
#3611 = EDGE_CURVE ( 'NONE', #6531, #7774, #2660, .T. ) ;
#3612 = DIRECTION ( 'NONE',  ( 0.000000000000000000, 1.000000000000000000, 0.000000000000000000 ) ) ;
#3613 = LINE ( 'NONE', #436, #1316 ) ;
#3614 = EDGE_LOOP ( 'NONE', ( #4842, #10369, #3076, #10449 ) ) ;
#3615 = AXIS2_PLACEMENT_3D ( 'NONE', #5348, #3718, #9334 ) ;
#3616 = ORIENTED_EDGE ( 'NONE', *, *, #169, .F. ) ;
#3617 = LINE ( 'NONE', #9286, #6084 ) ;
#3618 = ORIENTED_EDGE ( 'NONE', *, *, #10477, .F. ) ;
#3619 = ORIENTED_EDGE ( 'NONE', *, *, #5880, .T. ) ;
#3620 = FACE_BOUND ( 'NONE', #9058, .T. ) ;
#3621 = CARTESIAN_POINT ( 'NONE',  ( 10.26554134690924691, 64.37996872128307757, -7.750000000000000000 ) ) ;
#3622 = CIRCLE ( 'NONE', #2603, 7.525240063345735031 ) ;
#3623 = FACE_OUTER_BOUND ( 'NONE', #2986, .T. ) ;
#3624 = CARTESIAN_POINT ( 'NONE',  ( -1.071796769724492338, 3.592756407884963643, -1.758437202063677596 ) ) ;
#3625 = DIRECTION ( 'NONE',  ( -1.000000000000000000, 0.000000000000000000, 1.734723475976804383E-16 ) ) ;
#3626 =( REPRESENTATION_RELATIONSHIP ('NONE','NONE', #9007, #5747 ) REPRESENTATION_RELATIONSHIP_WITH_TRANSFORMATION ( #4789 )SHAPE_REPRESENTATION_RELATIONSHIP( ) );
#3627 = EDGE_LOOP ( 'NONE', ( #9969, #845, #2720, #1737 ) ) ;
#3628 = FACE_OUTER_BOUND ( 'NONE', #8929, .T. ) ;
#3629 = EDGE_CURVE ( 'NONE', #4419, #1304, #4379, .T. ) ;
#3630 = CIRCLE ( 'NONE', #4475, 2.000000000000001776 ) ;
#3631 = CARTESIAN_POINT ( 'NONE',  ( -20.29350689640809691, 140.5696653505793563, 19.97500000000000853 ) ) ;
#3632 = CARTESIAN_POINT ( 'NONE',  ( -31.74999999999995737, 3.673940397442060361E-16, -3.000000000000000444 ) ) ;
#3633 = VECTOR ( 'NONE', #2402, 1000.000000000000000 ) ;
#3634 = DIRECTION ( 'NONE',  ( -0.000000000000000000, 0.000000000000000000, -1.000000000000000000 ) ) ;
#3635 = CARTESIAN_POINT ( 'NONE',  ( 37.22759939293837306, -133.2806661801596420, 25.15769640663938489 ) ) ;
#3636 = FACE_OUTER_BOUND ( 'NONE', #4430, .T. ) ;
#3637 = PLANE ( 'NONE',  #7469 ) ;
#3638 = ORIENTED_EDGE ( 'NONE', *, *, #5713, .T. ) ;
#3639 = DIRECTION ( 'NONE',  ( 0.000000000000000000, 0.000000000000000000, -1.000000000000000000 ) ) ;
#3640 = ORIENTED_EDGE ( 'NONE', *, *, #6886, .F. ) ;
#3641 = DIRECTION ( 'NONE',  ( 0.000000000000000000, 0.000000000000000000, 1.000000000000000000 ) ) ;
#3642 = EDGE_CURVE ( 'NONE', #9384, #1692, #8503, .T. ) ;
#3643 = ORIENTED_EDGE ( 'NONE', *, *, #3269, .F. ) ;
#3644 = CIRCLE ( 'NONE', #4984, 2.000000000000001776 ) ;
#3645 = LINE ( 'NONE', #9317, #1810 ) ;
#3646 = EDGE_LOOP ( 'NONE', ( #6589, #3130, #5413, #7186 ) ) ;
#3647 = ORIENTED_EDGE ( 'NONE', *, *, #542, .T. ) ;
#3648 = LINE ( 'NONE', #10118, #7053 ) ;
#3649 = CARTESIAN_POINT ( 'NONE',  ( 38.19229777560031636, 37.08684478514405214, 12.50000000000000000 ) ) ;
#3650 = ORIENTED_EDGE ( 'NONE', *, *, #9181, .F. ) ;
#3651 = DIRECTION ( 'NONE',  ( 0.000000000000000000, 0.000000000000000000, 1.000000000000000000 ) ) ;
#3652 = FACE_BOUND ( 'NONE', #3826, .T. ) ;
#3653 = DIRECTION ( 'NONE',  ( -0.6691306063588566833, -0.7431448254773956874, 0.000000000000000000 ) ) ;
#3654 = AXIS2_PLACEMENT_3D ( 'NONE', #9310, #9253, #10050 ) ;
#3655 = ORIENTED_EDGE ( 'NONE', *, *, #2306, .T. ) ;
#3656 = EDGE_CURVE ( 'NONE', #2894, #426, #5349, .T. ) ;
#3657 = ORIENTED_EDGE ( 'NONE', *, *, #6508, .T. ) ;
#3658 = EDGE_CURVE ( 'NONE', #8983, #3675, #5363, .T. ) ;
#3659 = ADVANCED_FACE ( 'NONE', ( #7557 ), #9257, .T. ) ;
#3660 = DIRECTION ( 'NONE',  ( -0.6691306063588580155, -0.7431448254773944662, 0.000000000000000000 ) ) ;
#3661 = AXIS2_PLACEMENT_3D ( 'NONE', #9077, #8336, #135 ) ;
#3662 = ORIENTED_EDGE ( 'NONE', *, *, #300, .T. ) ;
#3663 = DIRECTION ( 'NONE',  ( -0.000000000000000000, -0.000000000000000000, 1.000000000000000000 ) ) ;
#3664 = DIRECTION ( 'NONE',  ( -1.000000000000000000, -0.000000000000000000, -0.000000000000000000 ) ) ;
#3665 = FACE_OUTER_BOUND ( 'NONE', #3217, .T. ) ;
#3666 = DIRECTION ( 'NONE',  ( 0.000000000000000000, 0.5735764363510470476, 0.8191520442889910214 ) ) ;
#3667 = ORIENTED_EDGE ( 'NONE', *, *, #5980, .F. ) ;
#3668 = CIRCLE ( 'NONE', #7062, 4.025000000000000355 ) ;
#3669 = ORIENTED_EDGE ( 'NONE', *, *, #1353, .F. ) ;
#3670 = EDGE_CURVE ( 'NONE', #2404, #5066, #3579, .T. ) ;
#3671 = ADVANCED_FACE ( 'NONE', ( #8453 ), #1192, .T. ) ;
#3672 = AXIS2_PLACEMENT_3D ( 'NONE', #8927, #8180, #8075 ) ;
#3673 = EDGE_CURVE ( 'NONE', #6943, #1359, #7133, .T. ) ;
#3674 = ORIENTED_EDGE ( 'NONE', *, *, #7437, .T. ) ;
#3675 = VERTEX_POINT ( 'NONE', #4689 ) ;
#3676 = DIRECTION ( 'NONE',  ( -0.000000000000000000, -0.000000000000000000, -1.000000000000000000 ) ) ;
#3677 = LINE ( 'NONE', #6795, #9681 ) ;
#3678 = CIRCLE ( 'NONE', #9612, 4.729641367753004921 ) ;
#3679 = CARTESIAN_POINT ( 'NONE',  ( -27.15769640663939555, -115.1457019118818863, -27.15769640663944173 ) ) ;
#3680 = ADVANCED_BREP_SHAPE_REPRESENTATION ( '', ( #2958, #4601 ), #1084 ) ;
#3681 = AXIS2_PLACEMENT_3D ( 'NONE', #227, #8432, #6191 ) ;
#3682 = AXIS2_PLACEMENT_3D ( 'NONE', #4950, #1620, #197 ) ;
#3683 = CARTESIAN_POINT ( 'NONE',  ( -55.94539818030328604, 129.0132282531173757, 3.999999999999992895 ) ) ;
#3684 = ORIENTED_EDGE ( 'NONE', *, *, #2170, .T. ) ;
#3685 = LINE ( 'NONE', #3469, #9543 ) ;
#3686 = EDGE_CURVE ( 'NONE', #6043, #9088, #7926, .T. ) ;
#3687 = CARTESIAN_POINT ( 'NONE',  ( 0.000000000000000000, -145.1457019118819005, -50.00000000000002132 ) ) ;
#3688 = AXIS2_PLACEMENT_3D ( 'NONE', #2703, #5089, #4142 ) ;
#3689 = ORIENTED_EDGE ( 'NONE', *, *, #2430, .F. ) ;
#3690 = EDGE_CURVE ( 'NONE', #289, #7867, #8557, .T. ) ;
#3691 = AXIS2_PLACEMENT_3D ( 'NONE', #2240, #8647, #4723 ) ;
#3692 = DIRECTION ( 'NONE',  ( -0.000000000000000000, 1.000000000000000000, -0.000000000000000000 ) ) ;
#3693 = DIRECTION ( 'NONE',  ( -1.000000000000000000, -0.000000000000000000, -0.000000000000000000 ) ) ;
#3694 = CARTESIAN_POINT ( 'NONE',  ( -115.3226892516804583, 225.1003166080523954, 0.000000000000000000 ) ) ;
#3695 = CARTESIAN_POINT ( 'NONE',  ( -16.29350689640809691, 76.32362273389503571, 4.729641367753004033 ) ) ;
#3696 = ORIENTED_EDGE ( 'NONE', *, *, #3008, .F. ) ;
#3697 = CARTESIAN_POINT ( 'NONE',  ( -30.29350689640809335, 80.56966535057935630, -20.00000000000000711 ) ) ;
#3698 = ORIENTED_EDGE ( 'NONE', *, *, #1554, .T. ) ;
#3699 = VERTEX_POINT ( 'NONE', #1297 ) ;
#3700 = CARTESIAN_POINT ( 'NONE',  ( -47.94539818030328604, 85.52895752738115220, -4.000000000000000000 ) ) ;
#3701 = ORIENTED_EDGE ( 'NONE', *, *, #8365, .T. ) ;
#3702 = ORIENTED_EDGE ( 'NONE', *, *, #7765, .T. ) ;
#3703 = CYLINDRICAL_SURFACE ( 'NONE', #3836, 4.999999999999996447 ) ;
#3704 = DIRECTION ( 'NONE',  ( 0.000000000000000000, 0.000000000000000000, 1.000000000000000000 ) ) ;
#3705 = EDGE_LOOP ( 'NONE', ( #5798, #10329, #6997, #7020 ) ) ;
#3706 = PLANE ( 'NONE',  #9034 ) ;
#3707 = CARTESIAN_POINT ( 'NONE',  ( -23.79350689640809335, 120.5289575273812233, -7.750000000000000000 ) ) ;
#3708 = CIRCLE ( 'NONE', #7424, 4.000000000000000000 ) ;
#3709 = PLANE ( 'NONE',  #4079 ) ;
#3710 = VERTEX_POINT ( 'NONE', #5319 ) ;
#3711 = VECTOR ( 'NONE', #1031, 1000.000000000000000 ) ;
#3712 = ORIENTED_EDGE ( 'NONE', *, *, #1976, .F. ) ;
#3713 = DIRECTION ( 'NONE',  ( 1.000000000000000000, -0.000000000000000000, -0.000000000000000000 ) ) ;
#3714 = ORIENTED_EDGE ( 'NONE', *, *, #9165, .F. ) ;
#3715 = DIRECTION ( 'NONE',  ( 0.000000000000000000, 0.000000000000000000, -1.000000000000000000 ) ) ;
#3716 = CARTESIAN_POINT ( 'NONE',  ( -21.29350689640810046, 105.5289575273812233, -10.90000000000000036 ) ) ;
#3717 = CIRCLE ( 'NONE', #1178, 2.000000000000001776 ) ;
#3718 = DIRECTION ( 'NONE',  ( -1.000000000000000000, -0.000000000000000000, -0.000000000000000000 ) ) ;
#3719 = EDGE_CURVE ( 'NONE', #9834, #4343, #665, .T. ) ;
#3720 = CARTESIAN_POINT ( 'NONE',  ( -7.293506896408097795, 126.8146633489777599, -25.00000000000000355 ) ) ;
#3721 = DIRECTION ( 'NONE',  ( -0.000000000000000000, -0.000000000000000000, -1.000000000000000000 ) ) ;
#3722 = ORIENTED_EDGE ( 'NONE', *, *, #5846, .F. ) ;
#3723 = ORIENTED_EDGE ( 'NONE', *, *, #4733, .F. ) ;
#3724 = CIRCLE ( 'NONE', #3855, 4.000000000000000000 ) ;
#3725 = ORIENTED_EDGE ( 'NONE', *, *, #1009, .F. ) ;
#3726 = ORIENTED_EDGE ( 'NONE', *, *, #5564, .T. ) ;
#3727 = DIRECTION ( 'NONE',  ( -0.000000000000000000, 0.000000000000000000, 1.000000000000000000 ) ) ;
#3728 = CARTESIAN_POINT ( 'NONE',  ( -56.36957570605427037, 137.0132282531173473, 0.000000000000000000 ) ) ;
#3729 = CARTESIAN_POINT ( 'NONE',  ( 10.26554134690924691, 90.52895752738122326, -7.750000000000000000 ) ) ;
#3730 = LINE ( 'NONE', #1972, #5285 ) ;
#3731 = ADVANCED_FACE ( 'NONE', ( #559 ), #10364, .T. ) ;
#3732 = ADVANCED_FACE ( 'NONE', ( #8771 ), #8716, .F. ) ;
#3733 = EDGE_CURVE ( 'NONE', #1166, #7910, #10259, .T. ) ;
#3734 = DIRECTION ( 'NONE',  ( 1.000000000000000000, -0.000000000000000000, -0.000000000000000000 ) ) ;
#3735 = EDGE_LOOP ( 'NONE', ( #6413, #7623, #2173, #5422, #9244 ) ) ;
#3736 = CARTESIAN_POINT ( 'NONE',  ( 59.99999999999999289, -145.1457019118819005, -40.00000000000000000 ) ) ;
#3737 = DIRECTION ( 'NONE',  ( -1.000000000000000000, 0.000000000000000000, 1.396588258780021135E-16 ) ) ;
#3738 = EDGE_CURVE ( 'NONE', #1083, #9488, #10156, .T. ) ;
#3739 = LINE ( 'NONE', #6972, #7917 ) ;
#3740 = FACE_OUTER_BOUND ( 'NONE', #3994, .T. ) ;
#3741 = CARTESIAN_POINT ( 'NONE',  ( -7.293506896408097795, 120.5696653505793705, 20.00000000000000711 ) ) ;
#3742 = VERTEX_POINT ( 'NONE', #5479 ) ;
#3743 = CARTESIAN_POINT ( 'NONE',  ( -7.293506896408097795, 120.5696653505793705, -28.00000000000000355 ) ) ;
#3744 = ORIENTED_EDGE ( 'NONE', *, *, #10147, .F. ) ;
#3745 = ORIENTED_EDGE ( 'NONE', *, *, #4405, .F. ) ;
#3746 = CARTESIAN_POINT ( 'NONE',  ( 3.000000000000000000, -1.467624384280024730, 2.542000000000003368 ) ) ;
#3747 = VERTEX_POINT ( 'NONE', #8610 ) ;
#3748 = AXIS2_PLACEMENT_3D ( 'NONE', #3621, #9344, #8386 ) ;
#3749 = VERTEX_POINT ( 'NONE', #8661 ) ;
#3750 = FACE_OUTER_BOUND ( 'NONE', #4998, .T. ) ;
#3751 = LINE ( 'NONE', #9536, #5778 ) ;
#3752 = EDGE_LOOP ( 'NONE', ( #6562, #7468 ) ) ;
#3753 = CARTESIAN_POINT ( 'NONE',  ( -7.293506896408097795, 88.56966535057934209, -20.00000000000001066 ) ) ;
#3754 = CARTESIAN_POINT ( 'NONE',  ( 23.76520584195949226, -145.1457019118819005, -97.78965767959371647 ) ) ;
#3755 = DIRECTION ( 'NONE',  ( 0.000000000000000000, 0.000000000000000000, -1.000000000000000000 ) ) ;
#3756 = CARTESIAN_POINT ( 'NONE',  ( -27.15769640663937778, -133.1457019118818721, -48.00000000000002132 ) ) ;
#3757 = CARTESIAN_POINT ( 'NONE',  ( -23.15769640663940976, -115.1457019118818863, 47.99999999999997868 ) ) ;
#3758 = CIRCLE ( 'NONE', #1552, 4.000000000000000000 ) ;
#3759 = VECTOR ( 'NONE', #2544, 1000.000000000000000 ) ;
#3760 = EDGE_CURVE ( 'NONE', #1079, #4081, #9522, .T. ) ;
#3761 = EDGE_CURVE ( 'NONE', #7686, #382, #6428, .T. ) ;
#3762 = ORIENTED_EDGE ( 'NONE', *, *, #6804, .T. ) ;
#3763 = CARTESIAN_POINT ( 'NONE',  ( -122.5292777575814114, 231.5891580443559121, 0.000000000000000000 ) ) ;
#3764 = ORIENTED_EDGE ( 'NONE', *, *, #7815, .T. ) ;
#3765 = CARTESIAN_POINT ( 'NONE',  ( -16.29350689640809691, -140.1746510883711778, 30.31717237747080773 ) ) ;
#3766 = CARTESIAN_POINT ( 'NONE',  ( 23.15769640663940265, -133.1457019118818721, -48.00000000000002132 ) ) ;
#3767 = CIRCLE ( 'NONE', #9695, 4.999999999999997335 ) ;
#3768 = ORIENTED_EDGE ( 'NONE', *, *, #7706, .T. ) ;
#3769 = CARTESIAN_POINT ( 'NONE',  ( 17.97972049165455388, 17.84145331825995484, -12.49999999999999289 ) ) ;
#3770 = CARTESIAN_POINT ( 'NONE',  ( -30.29350689640809335, 140.5696653505793563, 10.98204862120180003 ) ) ;
#3771 = LINE ( 'NONE', #9080, #9739 ) ;
#3772 = ORIENTED_EDGE ( 'NONE', *, *, #8402, .F. ) ;
#3773 = ORIENTED_EDGE ( 'NONE', *, *, #457, .F. ) ;
#3774 = AXIS2_PLACEMENT_3D ( 'NONE', #497, #9346, #7859 ) ;
#3775 = AXIS2_PLACEMENT_3D ( 'NONE', #7809, #5579, #1451 ) ;
#3776 = EDGE_CURVE ( 'NONE', #6574, #9783, #6167, .T. ) ;
#3777 = EDGE_LOOP ( 'NONE', ( #9685, #6029, #7830, #3039, #3444 ) ) ;
#3778 = EDGE_LOOP ( 'NONE', ( #766, #6098, #5752, #7906 ) ) ;
#3779 = DIRECTION ( 'NONE',  ( 0.000000000000000000, 1.000000000000000000, 0.000000000000000000 ) ) ;
#3780 = DIRECTION ( 'NONE',  ( -0.000000000000000000, -1.000000000000000000, -0.000000000000000000 ) ) ;
#3781 = LINE ( 'NONE', #3568, #1631 ) ;
#3782 = CARTESIAN_POINT ( 'NONE',  ( -7.293506896408097795, 2.445795361565304815E-15, 20.00000000000002132 ) ) ;
#3783 = AXIS2_PLACEMENT_3D ( 'NONE', #4610, #8799, #4663 ) ;
#3784 = CARTESIAN_POINT ( 'NONE',  ( -45.00000000000000000, 0.000000000000000000, 0.000000000000000000 ) ) ;
#3785 = VERTEX_POINT ( 'NONE', #9357 ) ;
#3786 = DIRECTION ( 'NONE',  ( 1.000000000000000000, 0.000000000000000000, 8.379529552680125332E-16 ) ) ;
#3787 = EDGE_CURVE ( 'NONE', #941, #4587, #3739, .T. ) ;
#3788 = EDGE_CURVE ( 'NONE', #7130, #3710, #9961, .T. ) ;
#3789 = AXIS2_PLACEMENT_3D ( 'NONE', #2592, #1689, #2534 ) ;
#3790 = ADVANCED_FACE ( 'NONE', ( #10318 ), #5374, .F. ) ;
#3791 = DIRECTION ( 'NONE',  ( 8.379529552680125332E-16, 0.000000000000000000, -1.000000000000000000 ) ) ;
#3792 = ORIENTED_EDGE ( 'NONE', *, *, #10398, .T. ) ;
#3793 = DIRECTION ( 'NONE',  ( 0.000000000000000000, -0.5660304919045651140, -0.8243843049417401980 ) ) ;
#3794 = CYLINDRICAL_SURFACE ( 'NONE', #1933, 3.297986701801175258 ) ;
#3795 = CARTESIAN_POINT ( 'NONE',  ( -40.00000000000002842, -145.1457019118819005, 43.99999999999997158 ) ) ;
#3796 = CIRCLE ( 'NONE', #6342, 7.500000000000000000 ) ;
#3797 = EDGE_LOOP ( 'NONE', ( #229, #7853, #3228, #2749 ) ) ;
#3798 = CARTESIAN_POINT ( 'NONE',  ( -155.4728935706336301, 261.2517229562222951, 0.000000000000000000 ) ) ;
#3799 = ORIENTED_EDGE ( 'NONE', *, *, #3328, .T. ) ;
#3800 = APPLICATION_PROTOCOL_DEFINITION ( 'draft international standard', 'automotive_design', 1998, #2265 ) ;
#3801 = ORIENTED_EDGE ( 'NONE', *, *, #6715, .F. ) ;
#3802 = EDGE_CURVE ( 'NONE', #4078, #1443, #4189, .T. ) ;
#3803 = DIRECTION ( 'NONE',  ( 0.000000000000000000, 0.000000000000000000, 1.000000000000000000 ) ) ;
#3804 = ORIENTED_EDGE ( 'NONE', *, *, #7322, .F. ) ;
#3805 = AXIS2_PLACEMENT_3D ( 'NONE', #4210, #3411, #7282 ) ;
#3806 = ORIENTED_EDGE ( 'NONE', *, *, #101, .F. ) ;
#3807 = DIRECTION ( 'NONE',  ( 0.000000000000000000, -0.4999999999999985567, 0.8660254037844394848 ) ) ;
#3808 = DIRECTION ( 'NONE',  ( -1.000000000000000000, 0.000000000000000000, 0.000000000000000000 ) ) ;
#3809 = DIRECTION ( 'NONE',  ( -0.6691306063588565722, -0.7431448254773957984, 0.000000000000000000 ) ) ;
#3810 = CARTESIAN_POINT ( 'NONE',  ( 27.15769640663936713, -115.1457019118818863, 27.15769640663938489 ) ) ;
#3811 = DIRECTION ( 'NONE',  ( 0.000000000000000000, 0.7071067811863512853, 0.7071067811867437491 ) ) ;
#3812 = DIRECTION ( 'NONE',  ( -1.000000000000000000, 0.000000000000000000, -1.396588258780018177E-16 ) ) ;
#3813 = FACE_OUTER_BOUND ( 'NONE', #9404, .T. ) ;
#3814 = CARTESIAN_POINT ( 'NONE',  ( -30.29350689640809335, 88.56966535057934209, 20.00000000000001066 ) ) ;
#3815 = CIRCLE ( 'NONE', #5156, 3.297986701801175258 ) ;
#3816 = VERTEX_POINT ( 'NONE', #6114 ) ;
#3817 = CARTESIAN_POINT ( 'NONE',  ( 3.000000000000000000, 2.935248768560057897, -3.252606517456513302E-15 ) ) ;
#3818 = AXIS2_PLACEMENT_3D ( 'NONE', #5760, #841, #3280 ) ;
#3819 = ORIENTED_EDGE ( 'NONE', *, *, #9237, .T. ) ;
#3820 = DIRECTION ( 'NONE',  ( -1.000000000000000000, 0.000000000000000000, 0.000000000000000000 ) ) ;
#3821 = CARTESIAN_POINT ( 'NONE',  ( -129.7734861572812974, 221.9362163441986411, 0.000000000000000000 ) ) ;
#3822 = DIRECTION ( 'NONE',  ( 0.000000000000000000, 0.000000000000000000, 1.000000000000000000 ) ) ;
#3823 = EDGE_CURVE ( 'NONE', #6283, #1352, #5884, .T. ) ;
#3824 = DIRECTION ( 'NONE',  ( 0.000000000000000000, -1.000000000000000000, 1.431206729101514631E-16 ) ) ;
#3825 = CARTESIAN_POINT ( 'NONE',  ( -16.29350689640809691, 105.5289575273812233, 54.43095569077609497 ) ) ;
#3826 = EDGE_LOOP ( 'NONE', ( #3391, #3168 ) ) ;
#3827 = VERTEX_POINT ( 'NONE', #9984 ) ;
#3828 = PRODUCT ( 'Metal Rod', 'Metal Rod', '', ( #10421 ) ) ;
#3829 = AXIS2_PLACEMENT_3D ( 'NONE', #3425, #4065, #9853 ) ;
#3830 = EDGE_LOOP ( 'NONE', ( #5465, #4515, #7641, #5821 ) ) ;
#3831 = EDGE_LOOP ( 'NONE', ( #743, #377, #7548, #3998, #6128, #388, #8707, #110, #8384, #2626 ) ) ;
#3832 = PLANE ( 'NONE',  #5211 ) ;
#3833 = CARTESIAN_POINT ( 'NONE',  ( -166.8975519277663295, 204.5843006325352746, -6.093437144708294610E-15 ) ) ;
#3834 = DIRECTION ( 'NONE',  ( 0.000000000000000000, 0.000000000000000000, 1.000000000000000000 ) ) ;
#3835 = FACE_OUTER_BOUND ( 'NONE', #1230, .T. ) ;
#3836 = AXIS2_PLACEMENT_3D ( 'NONE', #8466, #4336, #8415 ) ;
#3837 = EDGE_CURVE ( 'NONE', #8, #4758, #957, .T. ) ;
#3838 = CARTESIAN_POINT ( 'NONE',  ( -48.00000000000002132, -135.1457019118818721, 23.15769640663938134 ) ) ;
#3839 = AXIS2_PLACEMENT_3D ( 'NONE', #6429, #762, #7445 ) ;
#3840 = VERTEX_POINT ( 'NONE', #4295 ) ;
#3841 = CARTESIAN_POINT ( 'NONE',  ( -7.293506896408097795, 4.007378841484243628E-15, -28.00000000000002132 ) ) ;
#3842 = CIRCLE ( 'NONE', #8059, 7.862171649053781408 ) ;
#3843 = VERTEX_POINT ( 'NONE', #1753 ) ;
#3844 = CARTESIAN_POINT ( 'NONE',  ( -24.31850689640809549, 140.5696653505793563, 10.90000000000000036 ) ) ;
#3845 = VECTOR ( 'NONE', #10030, 1000.000000000000000 ) ;
#3846 = AXIS2_PLACEMENT_3D ( 'NONE', #8134, #1728, #8881 ) ;
#3847 = CARTESIAN_POINT ( 'NONE',  ( -11.29350689640809158, 105.5289575273812233, -25.04213562373096380 ) ) ;
#3848 = CARTESIAN_POINT ( 'NONE',  ( 73.53765631853929108, 70.39106037767955115, -25.00000000000000355 ) ) ;
#3849 = EDGE_CURVE ( 'NONE', #7537, #4871, #1700, .T. ) ;
#3850 = DIRECTION ( 'NONE',  ( -1.000000000000000000, 0.000000000000000000, 0.000000000000000000 ) ) ;
#3851 = VECTOR ( 'NONE', #1154, 1000.000000000000000 ) ;
#3852 = ADVANCED_FACE ( 'NONE', ( #279 ), #1861, .F. ) ;
#3853 = ORIENTED_EDGE ( 'NONE', *, *, #5767, .F. ) ;
#3854 = DIRECTION ( 'NONE',  ( 1.000000000000000000, 0.000000000000000000, -1.396588258780018177E-16 ) ) ;
#3855 = AXIS2_PLACEMENT_3D ( 'NONE', #2160, #7196, #3864 ) ;
#3856 = DIRECTION ( 'NONE',  ( 1.000000000000000000, 0.000000000000000000, 0.000000000000000000 ) ) ;
#3857 = ORIENTED_EDGE ( 'NONE', *, *, #1066, .T. ) ;
#3858 = CARTESIAN_POINT ( 'NONE',  ( -37.01000625782472753, 0.000000000000000000, 0.000000000000000000 ) ) ;
#3859 = ORIENTED_EDGE ( 'NONE', *, *, #6309, .T. ) ;
#3860 = TOROIDAL_SURFACE ( 'NONE', #8590, 4.000000000000000000, 2.000000000000000000 ) ;
#3861 = ORIENTED_EDGE ( 'NONE', *, *, #7879, .T. ) ;
#3862 = CARTESIAN_POINT ( 'NONE',  ( -30.29350689640809335, 72.56966535057935630, 20.00000000000001066 ) ) ;
#3863 = CARTESIAN_POINT ( 'NONE',  ( 39.99999999999997158, -135.1457019118818721, 35.97499999999998010 ) ) ;
#3864 = DIRECTION ( 'NONE',  ( 0.000000000000000000, 0.000000000000000000, 1.000000000000000000 ) ) ;
#3865 = CIRCLE ( 'NONE', #3171, 4.000000000000000000 ) ;
#3866 = DIRECTION ( 'NONE',  ( 0.000000000000000000, -0.000000000000000000, -1.000000000000000000 ) ) ;
#3867 = EDGE_CURVE ( 'NONE', #2739, #8380, #5828, .T. ) ;
#3868 = EDGE_CURVE ( 'NONE', #9316, #4943, #5198, .T. ) ;
#3869 = DIRECTION ( 'NONE',  ( 0.000000000000000000, 0.000000000000000000, -1.000000000000000000 ) ) ;
#3870 = ADVANCED_FACE ( 'NONE', ( #5773 ), #3448, .F. ) ;
#3871 = CARTESIAN_POINT ( 'NONE',  ( -2.293506896408097795, 152.5696653505793279, 30.00000000000000355 ) ) ;
#3872 = CARTESIAN_POINT ( 'NONE',  ( -113.6864418536728465, 239.8026890743979322, 1.472130188556198457E-15 ) ) ;
#3873 = AXIS2_PLACEMENT_3D ( 'NONE', #9544, #4707, #2636 ) ;
#3874 = AXIS2_PLACEMENT_3D ( 'NONE', #4933, #3514, #2711 ) ;
#3875 = ORIENTED_EDGE ( 'NONE', *, *, #677, .F. ) ;
#3876 = CARTESIAN_POINT ( 'NONE',  ( -20.29350689640809691, 140.5696653505793563, -10.98204862120179648 ) ) ;
#3877 = VERTEX_POINT ( 'NONE', #5931 ) ;
#3878 = CARTESIAN_POINT ( 'NONE',  ( -48.00000000000002132, -117.1457019118819005, 23.15769640663938134 ) ) ;
#3879 = DIRECTION ( 'NONE',  ( 0.000000000000000000, 0.000000000000000000, 1.000000000000000000 ) ) ;
#3880 = CIRCLE ( 'NONE', #4870, 7.500000000000000000 ) ;
#3881 = ORIENTED_EDGE ( 'NONE', *, *, #1213, .F. ) ;
#3882 = LINE ( 'NONE', #3974, #1912 ) ;
#3883 = CYLINDRICAL_SURFACE ( 'NONE', #7851, 4.000000000000000000 ) ;
#3884 = EDGE_CURVE ( 'NONE', #1994, #9911, #9173, .T. ) ;
#3885 = PLANE ( 'NONE',  #4656 ) ;
#3886 = ORIENTED_EDGE ( 'NONE', *, *, #5564, .F. ) ;
#3887 = ORIENTED_EDGE ( 'NONE', *, *, #995, .F. ) ;
#3888 = ADVANCED_FACE ( 'NONE', ( #8377 ), #6902, .F. ) ;
#3889 = ORIENTED_EDGE ( 'NONE', *, *, #2696, .T. ) ;
#3890 = AXIS2_PLACEMENT_3D ( 'NONE', #4947, #5112, #8345 ) ;
#3891 = ORIENTED_EDGE ( 'NONE', *, *, #1554, .F. ) ;
#3892 = LINE ( 'NONE', #8855, #7244 ) ;
#3893 = CARTESIAN_POINT ( 'NONE',  ( 24.15108826162069633, -134.0910007290636941, 49.99999999999998579 ) ) ;
#3894 = CARTESIAN_POINT ( 'NONE',  ( -57.23930847856152582, 167.4192747350194850, 0.000000000000000000 ) ) ;
#3895 = DIRECTION ( 'NONE',  ( 1.000000000000000000, -0.000000000000000000, -0.000000000000000000 ) ) ;
#3896 = LINE ( 'NONE', #7965, #4171 ) ;
#3897 = ORIENTED_EDGE ( 'NONE', *, *, #3656, .F. ) ;
#3898 = MECHANICAL_DESIGN_GEOMETRIC_PRESENTATION_REPRESENTATION (  '', ( #3380 ), #6255 ) ;
#3899 = CARTESIAN_POINT ( 'NONE',  ( -27.85255513972543895, 90.52895752738122326, 7.750000000000002665 ) ) ;
#3900 = EDGE_CURVE ( 'NONE', #9176, #5189, #1116, .T. ) ;
#3901 = ORIENTED_EDGE ( 'NONE', *, *, #5304, .T. ) ;
#3902 = CARTESIAN_POINT ( 'NONE',  ( -16.29350689640809691, 55.56966535057936341, 7.500000000000000000 ) ) ;
#3903 = DIRECTION ( 'NONE',  ( 0.1124875939035004102, -0.8191520442889910214, 0.5624379695174998028 ) ) ;
#3904 = LINE ( 'NONE', #9580, #424 ) ;
#3905 = LINE ( 'NONE', #1410, #7547 ) ;
#3906 = ORIENTED_EDGE ( 'NONE', *, *, #7396, .T. ) ;
#3907 = DIRECTION ( 'NONE',  ( 0.000000000000000000, -1.000000000000000000, 0.000000000000000000 ) ) ;
#3908 = APPLICATION_PROTOCOL_DEFINITION ( 'draft international standard', 'automotive_design', 1998, #8219 ) ;
#3909 = EDGE_LOOP ( 'NONE', ( #3616, #7241, #7180, #9613 ) ) ;
#3910 = CARTESIAN_POINT ( 'NONE',  ( -18.34874108452141783, -140.1746510883711778, -97.78965767959371647 ) ) ;
#3911 = EDGE_CURVE ( 'NONE', #10256, #1746, #134, .T. ) ;
#3912 = ORIENTED_EDGE ( 'NONE', *, *, #1220, .T. ) ;
#3913 = ORIENTED_EDGE ( 'NONE', *, *, #9379, .F. ) ;
#3914 = PLANE ( 'NONE',  #7214 ) ;
#3915 = SURFACE_SIDE_STYLE ('',( #6989 ) ) ;
#3916 = DIRECTION ( 'NONE',  ( -1.000000000000000000, 0.000000000000000000, 0.000000000000000000 ) ) ;
#3917 = CARTESIAN_POINT ( 'NONE',  ( -39.00428932080996702, -3.095342794014893428, -1.752073144804227933 ) ) ;
#3918 = DIRECTION ( 'NONE',  ( 0.000000000000000000, 1.000000000000000000, -0.000000000000000000 ) ) ;
#3919 = CARTESIAN_POINT ( 'NONE',  ( -7.293506896408097795, 72.56966535057935630, 20.00000000000001066 ) ) ;
#3920 = PRODUCT_DEFINITION_SHAPE ( 'NONE', 'NONE',  #687 ) ;
#3921 = ORIENTED_EDGE ( 'NONE', *, *, #6509, .T. ) ;
#3922 = DIRECTION ( 'NONE',  ( 0.000000000000000000, 0.000000000000000000, -1.000000000000000000 ) ) ;
#3923 = AXIS2_PLACEMENT_3D ( 'NONE', #7508, #3426, #256 ) ;
#3924 = EDGE_CURVE ( 'NONE', #1040, #2146, #9016, .T. ) ;
#3925 = EDGE_CURVE ( 'NONE', #2500, #4525, #2665, .T. ) ;
#3926 = EDGE_CURVE ( 'NONE', #3983, #9491, #2830, .T. ) ;
#3927 = ORIENTED_EDGE ( 'NONE', *, *, #7379, .F. ) ;
#3928 = DIRECTION ( 'NONE',  ( 3.469446951953611033E-15, -1.000000000000000000, 0.000000000000000000 ) ) ;
#3929 = CARTESIAN_POINT ( 'NONE',  ( -56.36957570605427748, 150.5696653505793563, 10.90000000000000036 ) ) ;
#3930 = LINE ( 'NONE', #7160, #1922 ) ;
#3931 = FACE_OUTER_BOUND ( 'NONE', #1363, .T. ) ;
#3932 = AXIS2_PLACEMENT_3D ( 'NONE', #6118, #3535, #2685 ) ;
#3933 = ORIENTED_EDGE ( 'NONE', *, *, #8965, .T. ) ;
#3934 = EDGE_LOOP ( 'NONE', ( #7042, #7343, #4080, #1301 ) ) ;
#3935 = AXIS2_PLACEMENT_3D ( 'NONE', #10224, #8073, #1609 ) ;
#3936 = ORIENTED_EDGE ( 'NONE', *, *, #2427, .T. ) ;
#3937 = EDGE_CURVE ( 'NONE', #3587, #4776, #9622, .T. ) ;
#3938 = AXIS2_PLACEMENT_3D ( 'NONE', #3186, #7170, #10454 ) ;
#3939 = DIRECTION ( 'NONE',  ( 1.000000000000000000, 1.277197683604454965E-16, -0.000000000000000000 ) ) ;
#3940 = LINE ( 'NONE', #7218, #6107 ) ;
#3941 = DIRECTION ( 'NONE',  ( 0.000000000000000000, -1.000000000000000000, 1.431206729101514631E-16 ) ) ;
#3942 = DIRECTION ( 'NONE',  ( 1.000000000000000000, 0.000000000000000000, 0.000000000000000000 ) ) ;
#3943 = CARTESIAN_POINT ( 'NONE',  ( 17.97972049165455388, 17.84145331825995484, 12.50000000000000355 ) ) ;
#3944 = AXIS2_PLACEMENT_3D ( 'NONE', #10404, #1448, #1550 ) ;
#3945 = VERTEX_POINT ( 'NONE', #2655 ) ;
#3946 = AXIS2_PLACEMENT_3D ( 'NONE', #6228, #2147, #3854 ) ;
#3947 = DIRECTION ( 'NONE',  ( 0.000000000000000000, -1.000000000000000000, -1.431206729101514631E-16 ) ) ;
#3948 = ORIENTED_EDGE ( 'NONE', *, *, #4048, .T. ) ;
#3949 = DIRECTION ( 'NONE',  ( 0.000000000000000000, -1.000000000000000000, 0.000000000000000000 ) ) ;
#3950 = UNCERTAINTY_MEASURE_WITH_UNIT (LENGTH_MEASURE( 1.000000000000000082E-05 ), #1688, 'distance_accuracy_value', 'NONE');
#3951 = AXIS2_PLACEMENT_3D ( 'NONE', #6581, #9824, #9015 ) ;
#3952 = CARTESIAN_POINT ( 'NONE',  ( 38.19229777560031636, 37.08684478514405214, -12.50000000000000000 ) ) ;
#3953 = EDGE_CURVE ( 'NONE', #289, #9495, #6582, .T. ) ;
#3954 = CARTESIAN_POINT ( 'NONE',  ( 6.250000000000005329, 3.980102097228898231E-16, 3.250000000000000444 ) ) ;
#3955 = ORIENTED_EDGE ( 'NONE', *, *, #8119, .T. ) ;
#3956 = CYLINDRICAL_SURFACE ( 'NONE', #3946, 2.000000000000001776 ) ;
#3957 = VECTOR ( 'NONE', #7464, 1000.000000000000000 ) ;
#3958 = APPLICATION_PROTOCOL_DEFINITION ( 'draft international standard', 'automotive_design', 1998, #4628 ) ;
#3959 = EDGE_LOOP ( 'NONE', ( #1776, #272, #2483, #1311, #1653 ) ) ;
#3960 = PLANE ( 'NONE',  #6916 ) ;
#3961 = EDGE_LOOP ( 'NONE', ( #10348, #2941, #9768, #9086 ) ) ;
#3962 = DIRECTION ( 'NONE',  ( 0.000000000000000000, -0.4309225046084501631, 0.9023889377768214981 ) ) ;
#3963 = FACE_OUTER_BOUND ( 'NONE', #363, .T. ) ;
#3964 = CARTESIAN_POINT ( 'NONE',  ( -16.29350689640809691, -186.9457019118818835, -7.500000000000000000 ) ) ;
#3965 = PLANE ( 'NONE',  #3135 ) ;
#3966 = CARTESIAN_POINT ( 'NONE',  ( 3.000000000000000000, -2.201436576420044755, -1.270999999999995911 ) ) ;
#3967 = CARTESIAN_POINT ( 'NONE',  ( -20.29350689640809691, 140.5696653505793563, 20.00000000000002132 ) ) ;
#3968 = EDGE_CURVE ( 'NONE', #7191, #7421, #3865, .T. ) ;
#3969 = ORIENTED_EDGE ( 'NONE', *, *, #1213, .T. ) ;
#3970 = CONICAL_SURFACE ( 'NONE', #8015, 4.000000000000003553, 1.029744258676655200 ) ;
#3971 = DIRECTION ( 'NONE',  ( -0.000000000000000000, 1.000000000000000000, -0.000000000000000000 ) ) ;
#3972 = ORIENTED_EDGE ( 'NONE', *, *, #8828, .T. ) ;
#3973 = CARTESIAN_POINT ( 'NONE',  ( -16.29350689640810401, 140.5696653505793563, 19.97500000000000853 ) ) ;
#3974 = CARTESIAN_POINT ( 'NONE',  ( -50.00000000000002842, -117.1457019118819005, 25.15769640663938134 ) ) ;
#3975 = CARTESIAN_POINT ( 'NONE',  ( -30.29350689640809335, 50.54838324668256888, 20.00000000000001776 ) ) ;
#3976 = AXIS2_PLACEMENT_3D ( 'NONE', #2355, #81, #137 ) ;
#3977 = DIRECTION ( 'NONE',  ( -0.7431448254773957984, 0.6691306063588565722, -0.000000000000000000 ) ) ;
#3978 = ORIENTED_EDGE ( 'NONE', *, *, #3367, .T. ) ;
#3979 = EDGE_CURVE ( 'NONE', #5311, #3827, #8594, .T. ) ;
#3980 = EDGE_CURVE ( 'NONE', #8969, #9987, #6222, .T. ) ;
#3981 = ORIENTED_EDGE ( 'NONE', *, *, #1380, .F. ) ;
#3982 = VECTOR ( 'NONE', #6774, 1000.000000000000000 ) ;
#3983 = VERTEX_POINT ( 'NONE', #9444 ) ;
#3984 = DIRECTION ( 'NONE',  ( -0.000000000000000000, -0.000000000000000000, 1.000000000000000000 ) ) ;
#3985 = FACE_OUTER_BOUND ( 'NONE', #4682, .T. ) ;
#3986 = AXIS2_PLACEMENT_3D ( 'NONE', #8732, #3112, #2368 ) ;
#3987 = CARTESIAN_POINT ( 'NONE',  ( -18.34874108452141783, -140.1746510883711778, -29.59847408863698703 ) ) ;
#3988 = CARTESIAN_POINT ( 'NONE',  ( -30.29350689640809335, 120.5696653505793705, -20.00000000000000711 ) ) ;
#3989 = PRODUCT_DEFINITION ( 'UNKNOWN', '', #2774, #8228 ) ;
#3990 = ADVANCED_FACE ( 'NONE', ( #8480 ), #4350, .T. ) ;
#3991 = DIRECTION ( 'NONE',  ( -0.6691306063588565722, -0.7431448254773956874, 0.000000000000000000 ) ) ;
#3992 = EDGE_CURVE ( 'NONE', #5268, #1057, #1960, .T. ) ;
#3993 = EDGE_CURVE ( 'NONE', #6699, #2463, #381, .T. ) ;
#3994 = EDGE_LOOP ( 'NONE', ( #1326, #5964, #298, #8127 ) ) ;
#3995 = AXIS2_PLACEMENT_3D ( 'NONE', #2578, #5805, #829 ) ;
#3996 = SHAPE_REPRESENTATION ( 'Reciprocating Punch Ram Shaft', ( #4601 ), #9900 ) ;
#3997 = EDGE_LOOP ( 'NONE', ( #1428, #2383, #6877, #4731 ) ) ;
#3998 = ORIENTED_EDGE ( 'NONE', *, *, #655, .T. ) ;
#3999 = DIRECTION ( 'NONE',  ( 1.000000000000000000, 0.000000000000000000, -1.137729606058012035E-16 ) ) ;
#4000 = AXIS2_PLACEMENT_3D ( 'NONE', #8569, #518, #5388 ) ;
#4001 = AXIS2_PLACEMENT_3D ( 'NONE', #7758, #3734, #2984 ) ;
#4002 = CARTESIAN_POINT ( 'NONE',  ( -144.3499457102809913, 273.6050080517225638, 2.035728505737848743E-15 ) ) ;
#4003 = CARTESIAN_POINT ( 'NONE',  ( 37.36731276015125758, -134.9005680707593342, -26.18936614083822434 ) ) ;
#4004 = EDGE_CURVE ( 'NONE', #5912, #5230, #533, .T. ) ;
#4005 = ORIENTED_EDGE ( 'NONE', *, *, #3402, .F. ) ;
#4006 = FACE_OUTER_BOUND ( 'NONE', #865, .T. ) ;
#4007 = CIRCLE ( 'NONE', #2475, 7.999999999999991118 ) ;
#4008 = ORIENTED_EDGE ( 'NONE', *, *, #804, .T. ) ;
#4009 = AXIS2_PLACEMENT_3D ( 'NONE', #1863, #5092, #8326 ) ;
#4010 = FACE_OUTER_BOUND ( 'NONE', #7372, .T. ) ;
#4011 = ORIENTED_EDGE ( 'NONE', *, *, #1711, .F. ) ;
#4012 = EDGE_CURVE ( 'NONE', #723, #1816, #1984, .T. ) ;
#4013 = ORIENTED_EDGE ( 'NONE', *, *, #10070, .F. ) ;
#4014 = VECTOR ( 'NONE', #4958, 1000.000000000000000 ) ;
#4015 = CARTESIAN_POINT ( 'NONE',  ( -16.29350689640809691, -115.1457019118818863, 0.000000000000000000 ) ) ;
#4016 = CARTESIAN_POINT ( 'NONE',  ( 14.70649310359190309, 120.5696653505793705, -24.00000000000000711 ) ) ;
#4017 = DIRECTION ( 'NONE',  ( -8.379529552680125332E-16, 0.000000000000000000, 1.000000000000000000 ) ) ;
#4018 = LINE ( 'NONE', #7188, #2382 ) ;
#4019 = AXIS2_PLACEMENT_3D ( 'NONE', #5221, #352, #2678 ) ;
#4020 = FACE_OUTER_BOUND ( 'NONE', #97, .T. ) ;
#4021 = ORIENTED_EDGE ( 'NONE', *, *, #4051, .F. ) ;
#4022 = AXIS2_PLACEMENT_3D ( 'NONE', #760, #8814, #7131 ) ;
#4023 = LINE ( 'NONE', #7254, #4351 ) ;
#4024 = AXIS2_PLACEMENT_3D ( 'NONE', #6523, #3292, #9773 ) ;
#4025 = VERTEX_POINT ( 'NONE', #1225 ) ;
#4026 = LINE ( 'NONE', #2477, #4209 ) ;
#4027 = CARTESIAN_POINT ( 'NONE',  ( 3.000000000000000000, 0.000000000000000000, 2.541999999999999815 ) ) ;
#4028 = CARTESIAN_POINT ( 'NONE',  ( -23.15769640663940621, -115.1457019118818863, 27.15769640663938489 ) ) ;
#4029 = DIRECTION ( 'NONE',  ( 0.000000000000000000, 1.000000000000000000, 0.000000000000000000 ) ) ;
#4030 = CARTESIAN_POINT ( 'NONE',  ( 27.15769640663936713, -133.1457019118818721, 27.15769640663938489 ) ) ;
#4031 = ORIENTED_EDGE ( 'NONE', *, *, #10339, .F. ) ;
#4032 = ORIENTED_EDGE ( 'NONE', *, *, #5381, .T. ) ;
#4033 = AXIS2_PLACEMENT_3D ( 'NONE', #8272, #5719, #116 ) ;
#4034 = ORIENTED_EDGE ( 'NONE', *, *, #5304, .F. ) ;
#4035 = EDGE_CURVE ( 'NONE', #6316, #2974, #650, .T. ) ;
#4036 = CARTESIAN_POINT ( 'NONE',  ( -50.00000000000002132, -134.0910177696405015, -24.15110854952568431 ) ) ;
#4037 = EDGE_CURVE ( 'NONE', #3587, #836, #3613, .T. ) ;
#4038 = CARTESIAN_POINT ( 'NONE',  ( -23.17384457509314544, 150.5696653505793563, -7.749999999999996447 ) ) ;
#4039 = CIRCLE ( 'NONE', #8094, 4.025000000000000355 ) ;
#4040 = DIRECTION ( 'NONE',  ( 0.000000000000000000, 0.000000000000000000, 1.000000000000000000 ) ) ;
#4041 = ORIENTED_EDGE ( 'NONE', *, *, #8365, .F. ) ;
#4042 = CARTESIAN_POINT ( 'NONE',  ( -30.29350689640809335, 80.56966535057935630, -16.00000000000000711 ) ) ;
#4043 = ORIENTED_EDGE ( 'NONE', *, *, #7223, .F. ) ;
#4044 = DIRECTION ( 'NONE',  ( 1.000000000000000000, -0.000000000000000000, -0.000000000000000000 ) ) ;
#4045 = AXIS2_PLACEMENT_3D ( 'NONE', #9883, #9070, #2501 ) ;
#4046 = VERTEX_POINT ( 'NONE', #9335 ) ;
#4047 = VERTEX_POINT ( 'NONE', #6040 ) ;
#4048 = EDGE_CURVE ( 'NONE', #5289, #9924, #5370, .T. ) ;
#4049 = DIRECTION ( 'NONE',  ( 1.000000000000000000, 0.000000000000000000, 0.000000000000000000 ) ) ;
#4050 = EDGE_CURVE ( 'NONE', #1239, #7344, #4529, .T. ) ;
#4051 = EDGE_CURVE ( 'NONE', #2146, #9349, #9449, .T. ) ;
#4052 = CARTESIAN_POINT ( 'NONE',  ( 17.97972049165455388, 42.08684478514406635, 30.00000000000000355 ) ) ;
#4053 = VECTOR ( 'NONE', #3223, 1000.000000000000000 ) ;
#4054 = DIRECTION ( 'NONE',  ( -0.000000000000000000, -1.000000000000000000, -0.000000000000000000 ) ) ;
#4055 = CARTESIAN_POINT ( 'NONE',  ( 37.24181578876673626, -134.1736247882644193, -25.42151319394753628 ) ) ;
#4056 = ORIENTED_EDGE ( 'NONE', *, *, #2503, .T. ) ;
#4057 = CARTESIAN_POINT ( 'NONE',  ( -3.173844575093148990, 105.5289575273812233, 10.90000000000000036 ) ) ;
#4058 = VERTEX_POINT ( 'NONE', #6842 ) ;
#4059 = CARTESIAN_POINT ( 'NONE',  ( 25.44550000000000978, 0.000000000000000000, 2.999999999999999556 ) ) ;
#4060 = EDGE_LOOP ( 'NONE', ( #3772, #140 ) ) ;
#4061 = ADVANCED_FACE ( 'NONE', ( #8637 ), #6783, .F. ) ;
#4062 = ORIENTED_EDGE ( 'NONE', *, *, #155, .T. ) ;
#4063 = DIRECTION ( 'NONE',  ( 0.000000000000000000, 0.000000000000000000, 1.000000000000000000 ) ) ;
#4064 = CYLINDRICAL_SURFACE ( 'NONE', #9209, 4.024999999999997691 ) ;
#4065 = DIRECTION ( 'NONE',  ( 0.000000000000000000, -1.000000000000000000, 0.000000000000000000 ) ) ;
#4066 = FACE_OUTER_BOUND ( 'NONE', #7268, .T. ) ;
#4067 = DIRECTION ( 'NONE',  ( -1.277197683604454965E-16, 1.000000000000000000, -0.000000000000000000 ) ) ;
#4068 = EDGE_LOOP ( 'NONE', ( #3881, #528, #844, #8698 ) ) ;
#4069 = FACE_OUTER_BOUND ( 'NONE', #2807, .T. ) ;
#4070 = ORIENTED_EDGE ( 'NONE', *, *, #9501, .F. ) ;
#4071 = DIRECTION ( 'NONE',  ( 0.000000000000000000, 0.000000000000000000, 1.000000000000000000 ) ) ;
#4072 = DIRECTION ( 'NONE',  ( -0.5000000000000051070, 0.000000000000000000, 0.8660254037844355990 ) ) ;
#4073 = LINE ( 'NONE', #8896, #1073 ) ;
#4074 = DIRECTION ( 'NONE',  ( -1.000000000000000000, -0.000000000000000000, -0.000000000000000000 ) ) ;
#4075 = CARTESIAN_POINT ( 'NONE',  ( -16.29350689640809691, -140.1746510883711778, -23.72119897386845722 ) ) ;
#4076 = VERTEX_POINT ( 'NONE', #2120 ) ;
#4077 = EDGE_CURVE ( 'NONE', #716, #1117, #3013, .T. ) ;
#4078 = VERTEX_POINT ( 'NONE', #333 ) ;
#4079 = AXIS2_PLACEMENT_3D ( 'NONE', #6940, #5339, #1319 ) ;
#4080 = ORIENTED_EDGE ( 'NONE', *, *, #7480, .F. ) ;
#4081 = VERTEX_POINT ( 'NONE', #3770 ) ;
#4082 = CARTESIAN_POINT ( 'NONE',  ( 27.15769640663937068, -135.1457019118818721, 47.99999999999997868 ) ) ;
#4083 = DIRECTION ( 'NONE',  ( 0.000000000000000000, -1.000000000000000000, 0.000000000000000000 ) ) ;
#4084 = VECTOR ( 'NONE', #3254, 1000.000000000000000 ) ;
#4085 = APPLICATION_CONTEXT ( 'automotive_design' ) ;
#4086 = VECTOR ( 'NONE', #1022, 999.9999999999998863 ) ;
#4087 = LINE ( 'NONE', #5883, #1413 ) ;
#4088 = CARTESIAN_POINT ( 'NONE',  ( -2.293506896408097795, -3.651280424770854409E-15, -24.99999999999998579 ) ) ;
#4089 = VERTEX_POINT ( 'NONE', #2016 ) ;
#4090 = CARTESIAN_POINT ( 'NONE',  ( -23.17384457509314899, 130.5696653505793847, -7.749999999999996447 ) ) ;
#4091 = ORIENTED_EDGE ( 'NONE', *, *, #7423, .F. ) ;
#4092 = DIRECTION ( 'NONE',  ( -0.000000000000000000, -0.000000000000000000, 1.000000000000000000 ) ) ;
#4093 = EDGE_CURVE ( 'NONE', #596, #8054, #3560, .T. ) ;
#4094 = MECHANICAL_DESIGN_GEOMETRIC_PRESENTATION_REPRESENTATION (  '', ( #5770 ), #379 ) ;
#4095 = CIRCLE ( 'NONE', #38, 3.999999999999993339 ) ;
#4096 = VERTEX_POINT ( 'NONE', #5985 ) ;
#4097 = UNCERTAINTY_MEASURE_WITH_UNIT (LENGTH_MEASURE( 1.000000000000000082E-05 ), #7158, 'distance_accuracy_value', 'NONE');
#4098 = DIRECTION ( 'NONE',  ( -0.000000000000000000, -0.000000000000000000, 1.000000000000000000 ) ) ;
#4099 =( NAMED_UNIT ( * ) PLANE_ANGLE_UNIT ( ) SI_UNIT ( $, .RADIAN. ) );
#4100 = DIRECTION ( 'NONE',  ( -1.277197683604454965E-16, 1.000000000000000000, 0.000000000000000000 ) ) ;
#4101 = AXIS2_PLACEMENT_3D ( 'NONE', #10014, #5176, #9265 ) ;
#4102 = VECTOR ( 'NONE', #3537, 1000.000000000000000 ) ;
#4103 = CARTESIAN_POINT ( 'NONE',  ( 37.59878849545336976, 32.08684478514406635, 12.50000000000000355 ) ) ;
#4104 = DIRECTION ( 'NONE',  ( 0.000000000000000000, 0.000000000000000000, 1.000000000000000000 ) ) ;
#4105 = ORIENTED_EDGE ( 'NONE', *, *, #4077, .T. ) ;
#4106 = CARTESIAN_POINT ( 'NONE',  ( -23.17384457509314899, 150.5696653505793563, 10.90000000000000036 ) ) ;
#4107 = ADVANCED_FACE ( 'NONE', ( #5246 ), #2863, .F. ) ;
#4108 = EDGE_CURVE ( 'NONE', #5466, #6943, #7744, .T. ) ;
#4109 = EDGE_CURVE ( 'NONE', #2019, #3592, #3, .T. ) ;
#4110 = ORIENTED_EDGE ( 'NONE', *, *, #8133, .F. ) ;
#4111 = TOROIDAL_SURFACE ( 'NONE', #3607, 20.00000000000001776, 4.000000000000000000 ) ;
#4112 = CYLINDRICAL_SURFACE ( 'NONE', #2855, 7.999999999999996447 ) ;
#4113 = CIRCLE ( 'NONE', #9188, 5.000000000000004441 ) ;
#4114 = ORIENTED_EDGE ( 'NONE', *, *, #1786, .F. ) ;
#4115 = PLANE ( 'NONE',  #8924 ) ;
#4116 = DIRECTION ( 'NONE',  ( 8.659560562356134638E-17, 0.7071067811864494290, -0.7071067811866454944 ) ) ;
#4117 = FACE_OUTER_BOUND ( 'NONE', #5987, .T. ) ;
#4118 = VECTOR ( 'NONE', #5192, 1000.000000000000000 ) ;
#4119 = CYLINDRICAL_SURFACE ( 'NONE', #8143, 4.999999999999995559 ) ;
#4120 = CARTESIAN_POINT ( 'NONE',  ( 59.99999999999997868, -135.1457019118818721, 30.00000000000000355 ) ) ;
#4121 = ADVANCED_FACE ( 'NONE', ( #5507 ), #4664, .F. ) ;
#4122 = ADVANCED_FACE ( 'NONE', ( #2284 ), #1826, .F. ) ;
#4123 = VERTEX_POINT ( 'NONE', #3177 ) ;
#4124 = DIRECTION ( 'NONE',  ( -0.000000000000000000, -0.000000000000000000, -1.000000000000000000 ) ) ;
#4125 = AXIS2_PLACEMENT_3D ( 'NONE', #6081, #521, #1104 ) ;
#4126 = ORIENTED_EDGE ( 'NONE', *, *, #5142, .F. ) ;
#4127 = CARTESIAN_POINT ( 'NONE',  ( -3.173844575093148990, 130.5696653505793847, 10.90000000000000036 ) ) ;
#4128 = CARTESIAN_POINT ( 'NONE',  ( 17.97972049165455388, 37.08684478514406635, -24.99999999999998934 ) ) ;
#4129 = DIRECTION ( 'NONE',  ( 0.000000000000000000, 0.000000000000000000, -1.000000000000000000 ) ) ;
#4130 = CARTESIAN_POINT ( 'NONE',  ( -38.99999999999999289, -5.592496027482437178E-16, 3.600000000000004530 ) ) ;
#4131 = CARTESIAN_POINT ( 'NONE',  ( 49.99999999999998579, -135.1457019118818721, -40.00000000000002132 ) ) ;
#4132 = FACE_BOUND ( 'NONE', #1864, .T. ) ;
#4133 = EDGE_LOOP ( 'NONE', ( #758, #6777, #8041, #4021 ) ) ;
#4134 = CIRCLE ( 'NONE', #6665, 4.000000000000000000 ) ;
#4135 = EDGE_LOOP ( 'NONE', ( #5860, #2924, #7204, #1357 ) ) ;
#4136 = VERTEX_POINT ( 'NONE', #4760 ) ;
#4137 = VERTEX_POINT ( 'NONE', #4611 ) ;
#4138 = CARTESIAN_POINT ( 'NONE',  ( -2.293506896408097795, 80.56966535057935630, 20.00000000000000711 ) ) ;
#4139 = ADVANCED_FACE ( 'NONE', ( #6257 ), #790, .F. ) ;
#4140 = CIRCLE ( 'NONE', #1267, 3.999999999999996447 ) ;
#4141 = CARTESIAN_POINT ( 'NONE',  ( -56.36957570605427037, 137.0132282531173473, 3.999999999999989786 ) ) ;
#4142 = DIRECTION ( 'NONE',  ( -0.6691306063588549069, -0.7431448254773971307, 0.000000000000000000 ) ) ;
#4143 = EDGE_LOOP ( 'NONE', ( #1791, #10399 ) ) ;
#4144 = CARTESIAN_POINT ( 'NONE',  ( 3.000000000000000000, -1.467624384280024730, 2.542000000000003368 ) ) ;
#4145 = ORIENTED_EDGE ( 'NONE', *, *, #8155, .T. ) ;
#4146 = CARTESIAN_POINT ( 'NONE',  ( -93.70792096198771048, 212.3425490925493762, 0.000000000000000000 ) ) ;
#4147 = AXIS2_PLACEMENT_3D ( 'NONE', #6569, #5132, #7520 ) ;
#4148 = ORIENTED_EDGE ( 'NONE', *, *, #3611, .F. ) ;
#4149 = AXIS2_PLACEMENT_3D ( 'NONE', #8366, #324, #1950 ) ;
#4150 = CARTESIAN_POINT ( 'NONE',  ( -7.293506896408097795, -3.651280424770854409E-15, -24.99999999999998579 ) ) ;
#4151 = LINE ( 'NONE', #3515, #3236 ) ;
#4152 = CARTESIAN_POINT ( 'NONE',  ( -30.29350689640809335, 2.445795361565304815E-15, -20.00000000000002132 ) ) ;
#4153 = DIRECTION ( 'NONE',  ( 0.000000000000000000, 0.000000000000000000, 1.000000000000000000 ) ) ;
#4154 = EDGE_CURVE ( 'NONE', #5439, #8294, #4814, .T. ) ;
#4155 = CARTESIAN_POINT ( 'NONE',  ( -158.4738950245593117, 241.4038491004292837, -2.052251677020569255E-15 ) ) ;
#4156 = CARTESIAN_POINT ( 'NONE',  ( 6.250000000000005329, 0.000000000000000000, 0.000000000000000000 ) ) ;
#4157 = AXIS2_PLACEMENT_3D ( 'NONE', #10228, #6082, #5131 ) ;
#4158 = ORIENTED_EDGE ( 'NONE', *, *, #10407, .T. ) ;
#4159 = DIRECTION ( 'NONE',  ( 0.000000000000000000, -0.000000000000000000, 1.000000000000000000 ) ) ;
#4160 = CONTEXT_DEPENDENT_SHAPE_REPRESENTATION ( #7475, #1459 ) ;
#4161 = ORIENTED_EDGE ( 'NONE', *, *, #5909, .T. ) ;
#4162 = CARTESIAN_POINT ( 'NONE',  ( 0.000000000000000000, -117.1457019118819005, -48.00000000000002132 ) ) ;
#4163 = ORIENTED_EDGE ( 'NONE', *, *, #1275, .F. ) ;
#4164 = ADVANCED_FACE ( 'NONE', ( #7955 ), #7903, .T. ) ;
#4165 = DIRECTION ( 'NONE',  ( -0.000000000000000000, 1.000000000000000000, -0.000000000000000000 ) ) ;
#4166 = FACE_OUTER_BOUND ( 'NONE', #6437, .T. ) ;
#4167 = DIRECTION ( 'NONE',  ( -1.000000000000000000, 0.000000000000000000, 0.000000000000000000 ) ) ;
#4168 = VECTOR ( 'NONE', #6267, 1000.000000000000000 ) ;
#4169 = DIRECTION ( 'NONE',  ( 0.000000000000000000, 0.000000000000000000, -1.000000000000000000 ) ) ;
#4170 = CARTESIAN_POINT ( 'NONE',  ( 94.78677303995212355, -145.1457019118819005, -30.00000000000000355 ) ) ;
#4171 = VECTOR ( 'NONE', #8652, 1000.000000000000000 ) ;
#4172 = ORIENTED_EDGE ( 'NONE', *, *, #1627, .T. ) ;
#4173 = LINE ( 'NONE', #7408, #4685 ) ;
#4174 = AXIS2_PLACEMENT_3D ( 'NONE', #4905, #9654, #835 ) ;
#4175 = ORIENTED_EDGE ( 'NONE', *, *, #7223, .T. ) ;
#4176 = DIRECTION ( 'NONE',  ( -0.000000000000000000, -0.000000000000000000, 1.000000000000000000 ) ) ;
#4177 = ADVANCED_FACE ( 'NONE', ( #10296 ), #7531, .T. ) ;
#4178 = CARTESIAN_POINT ( 'NONE',  ( -16.29350689640809691, -8.635287962196477096, -4.999999999999997335 ) ) ;
#4179 = EDGE_CURVE ( 'NONE', #6927, #8802, #2378, .T. ) ;
#4180 = AXIS2_PLACEMENT_3D ( 'NONE', #9670, #123, #3356 ) ;
#4181 = ADVANCED_FACE ( 'NONE', ( #7059 ), #693, .F. ) ;
#4182 = DIRECTION ( 'NONE',  ( -1.000000000000000000, 0.000000000000000000, 1.734723475976805615E-16 ) ) ;
#4183 = CARTESIAN_POINT ( 'NONE',  ( -16.29350689640809691, -115.1457019118818863, 7.500000000000000000 ) ) ;
#4184 = CARTESIAN_POINT ( 'NONE',  ( 1.940506014114294486E-14, -117.1457019118819005, -23.15769640663942752 ) ) ;
#4185 = PLANE ( 'NONE',  #4147 ) ;
#4186 = CLOSED_SHELL ( 'NONE', ( #8290, #4903, #3577, #5929, #5410, #4875, #9200, #8777, #3731, #2628, #4107, #4621, #706, #2022, #6521, #9219, #1529, #5745, #7164 ) ) ;
#4187 = ORIENTED_EDGE ( 'NONE', *, *, #8050, .F. ) ;
#4188 = EDGE_LOOP ( 'NONE', ( #7960, #1571, #4512, #5298 ) ) ;
#4189 = CIRCLE ( 'NONE', #7404, 4.729641367753003145 ) ;
#4190 = ORIENTED_EDGE ( 'NONE', *, *, #7208, .F. ) ;
#4191 = FACE_OUTER_BOUND ( 'NONE', #4940, .T. ) ;
#4192 = LINE ( 'NONE', #1807, #9868 ) ;
#4193 = VECTOR ( 'NONE', #9291, 1000.000000000000000 ) ;
#4194 = EDGE_CURVE ( 'NONE', #5490, #4722, #7874, .T. ) ;
#4195 = DIRECTION ( 'NONE',  ( 0.000000000000000000, -1.000000000000000000, 1.222897680782651224E-16 ) ) ;
#4196 = CARTESIAN_POINT ( 'NONE',  ( -2.293506896408097795, 80.56966535057935630, 20.00000000000000711 ) ) ;
#4197 = EDGE_LOOP ( 'NONE', ( #593, #6651, #537, #8794 ) ) ;
#4198 = DIRECTION ( 'NONE',  ( 1.000000000000000000, -0.000000000000000000, -0.000000000000000000 ) ) ;
#4199 = ORIENTED_EDGE ( 'NONE', *, *, #2360, .T. ) ;
#4200 = FILL_AREA_STYLE_COLOUR ( '', #6065 ) ;
#4201 = AXIS2_PLACEMENT_3D ( 'NONE', #6196, #5452, #4606 ) ;
#4202 = ORIENTED_EDGE ( 'NONE', *, *, #171, .F. ) ;
#4203 = CIRCLE ( 'NONE', #985, 8.000000000000000000 ) ;
#4204 = UNCERTAINTY_MEASURE_WITH_UNIT (LENGTH_MEASURE( 1.000000000000000082E-05 ), #520, 'distance_accuracy_value', 'NONE');
#4205 = DIRECTION ( 'NONE',  ( 0.000000000000000000, 0.000000000000000000, -1.000000000000000000 ) ) ;
#4206 = CARTESIAN_POINT ( 'NONE',  ( -16.29350689640809691, 65.65569765742554864, 4.729641367753004921 ) ) ;
#4207 = DIRECTION ( 'NONE',  ( 0.000000000000000000, 0.000000000000000000, 1.000000000000000000 ) ) ;
#4208 = LINE ( 'NONE', #2617, #8167 ) ;
#4209 = VECTOR ( 'NONE', #6453, 1000.000000000000000 ) ;
#4210 = CARTESIAN_POINT ( 'NONE',  ( -20.29350689640809691, 140.5696653505793563, 20.00000000000002132 ) ) ;
#4211 = DIRECTION ( 'NONE',  ( -0.000000000000000000, 1.000000000000000000, -0.000000000000000000 ) ) ;
#4212 = ORIENTED_EDGE ( 'NONE', *, *, #4733, .T. ) ;
#4213 = AXIS2_PLACEMENT_3D ( 'NONE', #5315, #1983, #1190 ) ;
#4214 = DIRECTION ( 'NONE',  ( -0.000000000000000000, -0.000000000000000000, 1.000000000000000000 ) ) ;
#4215 = EDGE_CURVE ( 'NONE', #6531, #10235, #6488, .T. ) ;
#4216 = APPLICATION_PROTOCOL_DEFINITION ( 'draft international standard', 'automotive_design', 1998, #5163 ) ;
#4217 = ORIENTED_EDGE ( 'NONE', *, *, #1064, .T. ) ;
#4218 = CARTESIAN_POINT ( 'NONE',  ( -30.29350689640809335, 80.56966535057935630, -20.00000000000000711 ) ) ;
#4219 = VERTEX_POINT ( 'NONE', #5609 ) ;
#4220 = MECHANICAL_DESIGN_GEOMETRIC_PRESENTATION_REPRESENTATION (  '', ( #9306 ), #1003 ) ;
#4221 = CARTESIAN_POINT ( 'NONE',  ( 27.15769640663936713, -135.1457019118818721, 27.15769640663938489 ) ) ;
#4222 = CARTESIAN_POINT ( 'NONE',  ( -40.00000000000002842, -135.1457019118818721, 35.97499999999998010 ) ) ;
#4223 = CYLINDRICAL_SURFACE ( 'NONE', #5329, 4.000000000000000000 ) ;
#4224 = VERTEX_POINT ( 'NONE', #5459 ) ;
#4225 = SURFACE_SIDE_STYLE ('',( #937 ) ) ;
#4226 = DIRECTION ( 'NONE',  ( 0.000000000000000000, 0.000000000000000000, 1.000000000000000000 ) ) ;
#4227 = ADVANCED_FACE ( 'NONE', ( #644 ), #3883, .F. ) ;
#4228 = VERTEX_POINT ( 'NONE', #3226 ) ;
#4229 = DIRECTION ( 'NONE',  ( 0.000000000000000000, -0.9374252720097653313, 0.3481865296036273372 ) ) ;
#4230 = ORIENTED_EDGE ( 'NONE', *, *, #2184, .T. ) ;
#4231 = CARTESIAN_POINT ( 'NONE',  ( -23.79350689640808980, 76.32362273389503571, -7.750000000000000000 ) ) ;
#4232 = CARTESIAN_POINT ( 'NONE',  ( -39.00436953563450970, -0.03089877619826558730, 3.555871974361681342 ) ) ;
#4233 = DIRECTION ( 'NONE',  ( -1.000000000000000000, 0.000000000000000000, 0.000000000000000000 ) ) ;
#4234 = DIRECTION ( 'NONE',  ( -0.000000000000000000, -1.000000000000000000, -0.000000000000000000 ) ) ;
#4235 = DIRECTION ( 'NONE',  ( -1.000000000000000000, 0.000000000000000000, 0.000000000000000000 ) ) ;
#4236 = ORIENTED_EDGE ( 'NONE', *, *, #4618, .F. ) ;
#4237 = EDGE_CURVE ( 'NONE', #10107, #477, #3930, .T. ) ;
#4238 = EDGE_CURVE ( 'NONE', #5439, #5589, #9609, .T. ) ;
#4239 = ORIENTED_EDGE ( 'NONE', *, *, #10239, .T. ) ;
#4240 = EDGE_CURVE ( 'NONE', #7054, #5162, #1541, .T. ) ;
#4241 = ORIENTED_EDGE ( 'NONE', *, *, #4929, .T. ) ;
#4242 = FACE_OUTER_BOUND ( 'NONE', #3735, .T. ) ;
#4243 = CARTESIAN_POINT ( 'NONE',  ( -47.94539818030330025, 137.0132282531173473, -3.999999999999991562 ) ) ;
#4244 = DIRECTION ( 'NONE',  ( -0.000000000000000000, 1.000000000000000000, -0.000000000000000000 ) ) ;
#4245 = VECTOR ( 'NONE', #4598, 1000.000000000000000 ) ;
#4246 = ORIENTED_EDGE ( 'NONE', *, *, #4093, .T. ) ;
#4247 = CARTESIAN_POINT ( 'NONE',  ( -40.33539666817951996, 3.418469287038280680, -2.079037510735945560 ) ) ;
#4248 = EDGE_LOOP ( 'NONE', ( #8890, #7075, #4673, #6353 ) ) ;
#4249 = DIRECTION ( 'NONE',  ( 0.000000000000000000, -1.224646799147353207E-16, 1.000000000000000000 ) ) ;
#4250 = PRODUCT_RELATED_PRODUCT_CATEGORY ( 'part', '', ( #8815 ) ) ;
#4251 = EDGE_LOOP ( 'NONE', ( #5455, #515, #8987 ) ) ;
#4252 = EDGE_CURVE ( 'NONE', #1613, #9607, #759, .T. ) ;
#4253 = ORIENTED_EDGE ( 'NONE', *, *, #8525, .T. ) ;
#4254 = LINE ( 'NONE', #6689, #5871 ) ;
#4255 =( NAMED_UNIT ( * ) SI_UNIT ( $, .STERADIAN. ) SOLID_ANGLE_UNIT ( ) );
#4256 = DIRECTION ( 'NONE',  ( -1.000000000000000000, 0.000000000000000000, 0.000000000000000000 ) ) ;
#4257 = CARTESIAN_POINT ( 'NONE',  ( -2.293506896408097795, 120.5696653505793705, 24.00000000000000711 ) ) ;
#4258 = FACE_OUTER_BOUND ( 'NONE', #1555, .T. ) ;
#4259 = CARTESIAN_POINT ( 'NONE',  ( -23.76520584195948516, -145.1457019118819005, 0.6509338422959615178 ) ) ;
#4260 = AXIS2_PLACEMENT_3D ( 'NONE', #2194, #6219, #1402 ) ;
#4261 = VERTEX_POINT ( 'NONE', #4910 ) ;
#4262 = CIRCLE ( 'NONE', #1727, 4.999999999999997335 ) ;
#4263 = DIRECTION ( 'NONE',  ( -1.396588258780021135E-16, 0.000000000000000000, -1.000000000000000000 ) ) ;
#4264 = EDGE_LOOP ( 'NONE', ( #913, #7746, #6785, #9673, #8190, #8904, #1504, #8985 ) ) ;
#4265 = DIRECTION ( 'NONE',  ( 0.000000000000000000, -1.000000000000000000, 0.000000000000000000 ) ) ;
#4266 = ORIENTED_EDGE ( 'NONE', *, *, #1427, .T. ) ;
#4267 = CIRCLE ( 'NONE', #1733, 7.499999999999996447 ) ;
#4268 =( BOUNDED_CURVE ( )  B_SPLINE_CURVE ( 3, ( #6344, #7828, #6130, #8674 ),
 .UNSPECIFIED., .F., .T. ) 
 B_SPLINE_CURVE_WITH_KNOTS ( ( 4, 4 ),
 ( 2.243596561310086113, 4.039588745869489017 ),
 .UNSPECIFIED. ) 
 CURVE ( )  GEOMETRIC_REPRESENTATION_ITEM ( )  RATIONAL_B_SPLINE_CURVE ( ( 1.000000000000000000, 0.7487856226529292503, 0.7487856226529292503, 1.000000000000000000 ) ) 
 REPRESENTATION_ITEM ( '' )  );
#4269 = ADVANCED_FACE ( 'NONE', ( #9109 ), #4634, .F. ) ;
#4270 = CARTESIAN_POINT ( 'NONE',  ( 94.78677303995212355, -145.1457019118819005, 30.00000000000000355 ) ) ;
#4271 = CARTESIAN_POINT ( 'NONE',  ( 14.70649310359190309, 80.56966535057935630, 20.00000000000000711 ) ) ;
#4272 = LINE ( 'NONE', #8194, #8046 ) ;
#4273 = CARTESIAN_POINT ( 'NONE',  ( 27.15769640663938489, -117.1457019118819005, -27.15769640663940976 ) ) ;
#4274 = CARTESIAN_POINT ( 'NONE',  ( -47.94539818030330025, 150.5696653505793563, 0.000000000000000000 ) ) ;
#4275 = AXIS2_PLACEMENT_3D ( 'NONE', #8441, #547, #8550 ) ;
#4276 = CIRCLE ( 'NONE', #6790, 5.000000000000004441 ) ;
#4277 = DIRECTION ( 'NONE',  ( 1.000000000000000000, 0.000000000000000000, 0.000000000000000000 ) ) ;
#4278 = ORIENTED_EDGE ( 'NONE', *, *, #1973, .F. ) ;
#4279 = CARTESIAN_POINT ( 'NONE',  ( -16.29350689640809691, -115.1457019118818863, -7.500000000000000000 ) ) ;
#4280 = EDGE_LOOP ( 'NONE', ( #7317, #130, #4013, #9753 ) ) ;
#4281 = DIRECTION ( 'NONE',  ( 1.000000000000000000, 0.000000000000000000, 0.000000000000000000 ) ) ;
#4282 = LINE ( 'NONE', #1157, #1897 ) ;
#4283 = DIRECTION ( 'NONE',  ( 0.000000000000000000, 0.000000000000000000, 1.000000000000000000 ) ) ;
#4284 = CARTESIAN_POINT ( 'NONE',  ( -2.293506896408097795, 145.5696653505793563, -25.00000000000000711 ) ) ;
#4285 = EDGE_CURVE ( 'NONE', #9459, #3359, #3339, .T. ) ;
#4286 = DIRECTION ( 'NONE',  ( -0.000000000000000000, -0.000000000000000000, -1.000000000000000000 ) ) ;
#4287 = DIRECTION ( 'NONE',  ( -1.000000000000000000, 0.000000000000000000, 0.000000000000000000 ) ) ;
#4288 = ORIENTED_EDGE ( 'NONE', *, *, #3204, .T. ) ;
#4289 = AXIS2_PLACEMENT_3D ( 'NONE', #2283, #1000, #4233 ) ;
#4290 = ORIENTED_EDGE ( 'NONE', *, *, #9363, .T. ) ;
#4291 = CARTESIAN_POINT ( 'NONE',  ( -40.99999999999999289, -5.556536133988210224E-16, 4.000000000000005329 ) ) ;
#4292 = CARTESIAN_POINT ( 'NONE',  ( -30.29350689640809335, 128.5696653505793563, -20.00000000000000711 ) ) ;
#4293 = CARTESIAN_POINT ( 'NONE',  ( 3.000000000000000000, 0.000000000000000000, 0.000000000000000000 ) ) ;
#4294 = EDGE_CURVE ( 'NONE', #2342, #4542, #5981, .T. ) ;
#4295 = CARTESIAN_POINT ( 'NONE',  ( 39.99999999999998579, -145.1457019118819005, -44.00000000000001421 ) ) ;
#4296 = AXIS2_PLACEMENT_3D ( 'NONE', #5004, #8247, #4951 ) ;
#4297 = ADVANCED_FACE ( 'NONE', ( #6671 ), #6567, .T. ) ;
#4298 = ORIENTED_EDGE ( 'NONE', *, *, #1052, .T. ) ;
#4299 = CARTESIAN_POINT ( 'NONE',  ( -39.65557114539780059, 3.370159726842552050, -2.156467633200104483 ) ) ;
#4300 = AXIS2_PLACEMENT_3D ( 'NONE', #1150, #3481, #362 ) ;
#4301 = ORIENTED_EDGE ( 'NONE', *, *, #817, .F. ) ;
#4302 = CARTESIAN_POINT ( 'NONE',  ( -163.6191320026764231, 264.0413720900392036, 0.000000000000000000 ) ) ;
#4303 = AXIS2_PLACEMENT_3D ( 'NONE', #10260, #1355, #2938 ) ;
#4304 = ORIENTED_EDGE ( 'NONE', *, *, #5557, .T. ) ;
#4305 = CARTESIAN_POINT ( 'NONE',  ( 6.756858349438843447, 146.7073643690756057, 30.00000000000000355 ) ) ;
#4306 = DIRECTION ( 'NONE',  ( -0.000000000000000000, 1.000000000000000000, -0.000000000000000000 ) ) ;
#4307 = CARTESIAN_POINT ( 'NONE',  ( 27.15769640663938489, -115.1457019118818863, -23.15769640663940976 ) ) ;
#4308 = DIRECTION ( 'NONE',  ( -0.6691306063588562392, -0.7431448254773960205, 0.000000000000000000 ) ) ;
#4309 = EDGE_CURVE ( 'NONE', #4219, #4136, #8379, .T. ) ;
#4310 = EDGE_CURVE ( 'NONE', #3419, #8839, #6003, .T. ) ;
#4311 = EDGE_CURVE ( 'NONE', #172, #541, #5323, .T. ) ;
#4312 = CARTESIAN_POINT ( 'NONE',  ( -51.94539818030329315, 155.5289575273811522, -4.898587196589407898E-16 ) ) ;
#4313 = DIRECTION ( 'NONE',  ( -0.7367503238654704578, 0.6761648913424330720, 0.000000000000000000 ) ) ;
#4314 = AXIS2_PLACEMENT_3D ( 'NONE', #9610, #2338, #4762 ) ;
#4315 = EDGE_LOOP ( 'NONE', ( #9603, #3065, #9285 ) ) ;
#4316 = CYLINDRICAL_SURFACE ( 'NONE', #2922, 3.999999999999989786 ) ;
#4317 = AXIS2_PLACEMENT_3D ( 'NONE', #1105, #5338, #7782 ) ;
#4318 = VERTEX_POINT ( 'NONE', #9813 ) ;
#4319 = CARTESIAN_POINT ( 'NONE',  ( 0.000000000000000000, 0.000000000000000000, 0.000000000000000000 ) ) ;
#4320 = ORIENTED_EDGE ( 'NONE', *, *, #6959, .F. ) ;
#4321 =( NAMED_UNIT ( * ) SI_UNIT ( $, .STERADIAN. ) SOLID_ANGLE_UNIT ( ) );
#4322 = CONICAL_SURFACE ( 'NONE', #4665, 4.025000000000000355, 0.7853981633973787790 ) ;
#4323 = ADVANCED_FACE ( 'NONE', ( #8310 ), #1048, .T. ) ;
#4324 = DIRECTION ( 'NONE',  ( 0.000000000000000000, 0.000000000000000000, 1.000000000000000000 ) ) ;
#4325 = DIRECTION ( 'NONE',  ( 0.000000000000000000, 0.000000000000000000, 1.000000000000000000 ) ) ;
#4326 = DIRECTION ( 'NONE',  ( 0.000000000000000000, -0.5000000000000011102, -0.8660254037844379305 ) ) ;
#4327 = CARTESIAN_POINT ( 'NONE',  ( -7.293506896408097795, 0.000000000000000000, 0.000000000000000000 ) ) ;
#4328 = VERTEX_POINT ( 'NONE', #3491 ) ;
#4329 = DIRECTION ( 'NONE',  ( 1.000000000000000000, -0.000000000000000000, -0.000000000000000000 ) ) ;
#4330 = CARTESIAN_POINT ( 'NONE',  ( 0.000000000000000000, 0.000000000000000000, 0.000000000000000000 ) ) ;
#4331 = EDGE_CURVE ( 'NONE', #3508, #3054, #9914, .T. ) ;
#4332 = EDGE_LOOP ( 'NONE', ( #8016, #10231, #6035, #2761 ) ) ;
#4333 = AXIS2_PLACEMENT_3D ( 'NONE', #2886, #1936, #6117 ) ;
#4334 = CARTESIAN_POINT ( 'NONE',  ( -54.56278605312608931, 170.3918540369290895, 0.000000000000000000 ) ) ;
#4335 = ORIENTED_EDGE ( 'NONE', *, *, #7994, .T. ) ;
#4336 = DIRECTION ( 'NONE',  ( -0.07334937666141726209, 0.9973063064792991872, 0.000000000000000000 ) ) ;
#4337 = CARTESIAN_POINT ( 'NONE',  ( 27.15769640663938489, -133.1457019118818721, -27.15769640663940976 ) ) ;
#4338 = CIRCLE ( 'NONE', #7377, 3.999999999999993339 ) ;
#4339 = DIRECTION ( 'NONE',  ( -1.000000000000000000, 0.000000000000000000, 0.000000000000000000 ) ) ;
#4340 = CYLINDRICAL_SURFACE ( 'NONE', #4317, 10.00000000000000000 ) ;
#4341 = VECTOR ( 'NONE', #4573, 1000.000000000000000 ) ;
#4342 = DIRECTION ( 'NONE',  ( 0.000000000000000000, 0.000000000000000000, -1.000000000000000000 ) ) ;
#4343 = VERTEX_POINT ( 'NONE', #2695 ) ;
#4344 = ORIENTED_EDGE ( 'NONE', *, *, #2245, .T. ) ;
#4345 = VECTOR ( 'NONE', #1374, 1000.000000000000000 ) ;
#4346 = CIRCLE ( 'NONE', #10443, 7.500000000000000000 ) ;
#4347 = ORIENTED_EDGE ( 'NONE', *, *, #1233, .T. ) ;
#4348 = LINE ( 'NONE', #7741, #3529 ) ;
#4349 = CARTESIAN_POINT ( 'NONE',  ( -50.00000000000001421, -133.3869996355352612, 23.39899473323094270 ) ) ;
#4350 = PLANE ( 'NONE',  #312 ) ;
#4351 = VECTOR ( 'NONE', #3219, 1000.000000000000000 ) ;
#4352 = EDGE_LOOP ( 'NONE', ( #2539, #4304, #8852, #4892 ) ) ;
#4353 = LINE ( 'NONE', #9932, #5011 ) ;
#4354 = ORIENTED_EDGE ( 'NONE', *, *, #1888, .F. ) ;
#4355 = CIRCLE ( 'NONE', #5021, 7.500000000000000000 ) ;
#4356 = CARTESIAN_POINT ( 'NONE',  ( 0.3000000000000016542, 5.755839955992559655E-16, -4.700000000000000178 ) ) ;
#4357 = EDGE_CURVE ( 'NONE', #4343, #3877, #3470, .T. ) ;
#4358 = AXIS2_PLACEMENT_3D ( 'NONE', #3872, #8887, #7837 ) ;
#4359 = CLOSED_SHELL ( 'NONE', ( #570, #7878, #6208, #9860, #857, #7865, #4139, #616, #2359, #1611, #10351, #4888, #4743, #9567, #3888, #8424, #8714, #8844, #4684, #6762, #1759, #3606, #529, #1901, #4563, #6970, #180, #30, #5472, #2811, #4846, #9628, #3331, #4323, #3732, #3553, #5399, #9690, #6969, #6687, #7252, #3346, #3990, #5024, #3539, #10015, #8672, #580, #5441, #2738, #5395, #9483, #6108, #1261, #1338, #1569, #9965, #8065, #3399, #5238, #7805, #1995, #4122, #5525, #5081, #6380, #9752, #8493, #10341, #1806, #2351, #5754, #1350, #8888, #8902, #7762, #9828, #10452, #1657, #6411, #6946, #5157, #4992, #4181, #9352, #7221, #2361, #6026, #4227, #870, #3051, #5237, #4695, #5652, #8727, #10467, #936, #4389, #9803, #2045, #8816, #9290, #1582, #2753, #7232, #1726, #9243, #6109, #3080, #1335, #4966, #1470, #949, #9627, #9407, #4297, #9231, #5699, #6899, #10025, #7852, #3195, #9599, #9039, #7287, #6836, #921, #6171, #8037, #6187, #223, #2825, #3463, #196, #64, #6263, #3432, #9766, #9081, #10261, #8391, #2880, #1396, #4562, #4574, #7482, #8906, #6392 ) ) ;
#4360 = VERTEX_POINT ( 'NONE', #5709 ) ;
#4361 = VERTEX_POINT ( 'NONE', #9003 ) ;
#4362 = DIRECTION ( 'NONE',  ( 0.000000000000000000, 1.222897680782651471E-16, 1.000000000000000000 ) ) ;
#4363 = CARTESIAN_POINT ( 'NONE',  ( 5.999999999999998224, 0.000000000000000000, 5.000000000000000000 ) ) ;
#4364 = VECTOR ( 'NONE', #9825, 1000.000000000000114 ) ;
#4365 = DIRECTION ( 'NONE',  ( 1.000000000000000000, 0.000000000000000000, 0.000000000000000000 ) ) ;
#4366 = UNCERTAINTY_MEASURE_WITH_UNIT (LENGTH_MEASURE( 1.000000000000000082E-05 ), #8417, 'distance_accuracy_value', 'NONE');
#4367 = CARTESIAN_POINT ( 'NONE',  ( 77.30044127146538813, 73.68369600860394542, 12.50000000000000000 ) ) ;
#4368 = DIRECTION ( 'NONE',  ( 0.000000000000000000, 0.7071067811865420216, 0.7071067811865531239 ) ) ;
#4369 = AXIS2_PLACEMENT_3D ( 'NONE', #4872, #6622, #902 ) ;
#4370 = ORIENTED_EDGE ( 'NONE', *, *, #387, .T. ) ;
#4371 = FACE_OUTER_BOUND ( 'NONE', #4135, .T. ) ;
#4372 = EDGE_CURVE ( 'NONE', #8917, #6578, #5664, .T. ) ;
#4374 = EDGE_CURVE ( 'NONE', #59, #7038, #8100, .T. ) ;
#4373 = VERTEX_POINT ( 'NONE', #4864 ) ;
#4375 = EDGE_CURVE ( 'NONE', #1149, #2894, #1797, .T. ) ;
#4376 = FACE_OUTER_BOUND ( 'NONE', #2798, .T. ) ;
#4377 = VERTEX_POINT ( 'NONE', #895 ) ;
#4378 = VECTOR ( 'NONE', #1273, 1000.000000000000000 ) ;
#4379 = LINE ( 'NONE', #8348, #9954 ) ;
#4380 = AXIS2_PLACEMENT_3D ( 'NONE', #2262, #8670, #3105 ) ;
#4381 = CARTESIAN_POINT ( 'NONE',  ( -36.36957570605426326, 137.0132282531173473, 0.000000000000000000 ) ) ;
#4382 = LINE ( 'NONE', #5266, #7709 ) ;
#4383 = CARTESIAN_POINT ( 'NONE',  ( -38.96131932220313132, -3.319229491889264416, -2.232199717805851691 ) ) ;
#4384 = ORIENTED_EDGE ( 'NONE', *, *, #2895, .F. ) ;
#4385 = DIRECTION ( 'NONE',  ( 0.000000000000000000, 1.222897680782651471E-16, 1.000000000000000000 ) ) ;
#4386 = VERTEX_POINT ( 'NONE', #4131 ) ;
#4387 =( NAMED_UNIT ( * ) SI_UNIT ( $, .STERADIAN. ) SOLID_ANGLE_UNIT ( ) );
#4388 = ORIENTED_EDGE ( 'NONE', *, *, #7256, .F. ) ;
#4389 = ADVANCED_FACE ( 'NONE', ( #8209 ), #6616, .T. ) ;
#4390 = FACE_OUTER_BOUND ( 'NONE', #6470, .T. ) ;
#4391 = AXIS2_PLACEMENT_3D ( 'NONE', #2034, #1241, #8499 ) ;
#4392 = ORIENTED_EDGE ( 'NONE', *, *, #2609, .T. ) ;
#4393 = CARTESIAN_POINT ( 'NONE',  ( -48.00000000000002132, -115.1457019118818863, -6.661338147750942398E-15 ) ) ;
#4394 = CARTESIAN_POINT ( 'NONE',  ( -7.293506896408097795, -0.3998014571812398832, 1.076388538564875708 ) ) ;
#4395 = B_SPLINE_CURVE_WITH_KNOTS ( 'NONE', 3,
 ( #9087, #8242, #5000, #7395, #4896, #7342, #8986, #1673, #2572, #872 ),
 .UNSPECIFIED., .F., .F.,
 ( 4, 2, 2, 2, 4 ),
 ( -8.944271910636758738E-06, 0.001019331502940711920, 0.002047607277792060521, 0.003075883052643409339, 0.004104158827494757723 ),
 .UNSPECIFIED. ) ;
#4396 = CARTESIAN_POINT ( 'NONE',  ( -2.293506896408097795, 80.56966535057935630, -20.00000000000000711 ) ) ;
#4397 = PLANE ( 'NONE',  #4149 ) ;
#4398 = CARTESIAN_POINT ( 'NONE',  ( -2.293506896408097795, 80.56966535057935630, -24.00000000000000711 ) ) ;
#4399 = AXIS2_PLACEMENT_3D ( 'NONE', #4441, #1263, #9267 ) ;
#4400 = VERTEX_POINT ( 'NONE', #1001 ) ;
#4401 = ORIENTED_EDGE ( 'NONE', *, *, #6630, .T. ) ;
#4402 = ORIENTED_EDGE ( 'NONE', *, *, #993, .F. ) ;
#4403 = CARTESIAN_POINT ( 'NONE',  ( 0.000000000000000000, -117.1457019118819005, 23.15769640663938134 ) ) ;
#4404 = CARTESIAN_POINT ( 'NONE',  ( -50.00000000000002132, -133.1457019118818721, 23.15769640663938134 ) ) ;
#4405 = EDGE_CURVE ( 'NONE', #719, #9924, #5818, .T. ) ;
#4406 = CARTESIAN_POINT ( 'NONE',  ( -16.29350689640809691, -7.660287962196459688, 0.000000000000000000 ) ) ;
#4407 = VERTEX_POINT ( 'NONE', #5922 ) ;
#4408 = CARTESIAN_POINT ( 'NONE',  ( 4.856471286862175774, 147.5696653505793279, 30.00000000000000355 ) ) ;
#4409 = ORIENTED_EDGE ( 'NONE', *, *, #428, .T. ) ;
#4410 = ORIENTED_EDGE ( 'NONE', *, *, #9461, .F. ) ;
#4411 = CARTESIAN_POINT ( 'NONE',  ( 0.3000000000000016542, 0.000000000000000000, 5.000000000000000000 ) ) ;
#4412 = DIRECTION ( 'NONE',  ( -0.000000000000000000, -1.000000000000000000, -0.000000000000000000 ) ) ;
#4413 = DIRECTION ( 'NONE',  ( -0.000000000000000000, -1.000000000000000000, -0.000000000000000000 ) ) ;
#4414 = ADVANCED_FACE ( 'NONE', ( #8574 ), #4397, .T. ) ;
#4415 = DIRECTION ( 'NONE',  ( 0.000000000000000000, 0.000000000000000000, 1.000000000000000000 ) ) ;
#4416 = EDGE_LOOP ( 'NONE', ( #6142, #3010, #4145, #1095, #10153, #9819, #3055, #6388, #3078, #9041, #7776, #5214 ) ) ;
#4417 = DIRECTION ( 'NONE',  ( 8.659560562357336419E-17, 0.7071067811863512853, -0.7071067811867437491 ) ) ;
#4418 = AXIS2_PLACEMENT_3D ( 'NONE', #1371, #8788, #10433 ) ;
#4419 = VERTEX_POINT ( 'NONE', #8470 ) ;
#4420 = CARTESIAN_POINT ( 'NONE',  ( -3.173844575093148990, 105.5289575273812233, 10.90000000000000036 ) ) ;
#4421 = EDGE_LOOP ( 'NONE', ( #6149, #8118, #539, #375 ) ) ;
#4422 = VECTOR ( 'NONE', #4860, 1000.000000000000114 ) ;
#4423 = DIRECTION ( 'NONE',  ( -0.000000000000000000, 1.000000000000000000, -0.000000000000000000 ) ) ;
#4424 = CARTESIAN_POINT ( 'NONE',  ( -30.29350689640809335, 80.56966535057935630, 20.00000000000000711 ) ) ;
#4425 = EDGE_CURVE ( 'NONE', #5689, #2102, #7627, .T. ) ;
#4426 = FACE_OUTER_BOUND ( 'NONE', #4188, .T. ) ;
#4427 = EDGE_CURVE ( 'NONE', #8618, #9366, #9377, .T. ) ;
#4428 = ADVANCED_FACE ( 'NONE', ( #3550 ), #4340, .T. ) ;
#4429 = CARTESIAN_POINT ( 'NONE',  ( -3.173844575093148990, 105.5289575273812233, -7.750000000000000000 ) ) ;
#4430 = EDGE_LOOP ( 'NONE', ( #9412, #7534, #9123, #2319 ) ) ;
#4431 = DIRECTION ( 'NONE',  ( -0.000000000000000000, -0.000000000000000000, -1.000000000000000000 ) ) ;
#4432 = VERTEX_POINT ( 'NONE', #10019 ) ;
#4433 = ORIENTED_EDGE ( 'NONE', *, *, #4646, .F. ) ;
#4434 = AXIS2_PLACEMENT_3D ( 'NONE', #2692, #7571, #321 ) ;
#4435 = DIRECTION ( 'NONE',  ( 0.000000000000000000, 0.000000000000000000, -1.000000000000000000 ) ) ;
#4436 = VECTOR ( 'NONE', #1392, 1000.000000000000000 ) ;
#4437 = VERTEX_POINT ( 'NONE', #10173 ) ;
#4438 = CARTESIAN_POINT ( 'NONE',  ( -40.00000000000002842, -115.1457019118818863, 39.99999999999997868 ) ) ;
#4439 = DIRECTION ( 'NONE',  ( 0.000000000000000000, 1.000000000000000000, 0.000000000000000000 ) ) ;
#4440 = ORIENTED_EDGE ( 'NONE', *, *, #8077, .T. ) ;
#4441 = CARTESIAN_POINT ( 'NONE',  ( -1.071796769724492338, 0.000000000000000000, 0.000000000000000000 ) ) ;
#4442 = DIRECTION ( 'NONE',  ( 0.000000000000000000, 0.000000000000000000, 1.000000000000000000 ) ) ;
#4443 = PRODUCT_RELATED_PRODUCT_CATEGORY ( 'part', '', ( #9406 ) ) ;
#4444 = EDGE_CURVE ( 'NONE', #5509, #9513, #8883, .T. ) ;
#4445 = CARTESIAN_POINT ( 'NONE',  ( 80.08610854271792334, 54.73418909528891874, -25.00000000000000355 ) ) ;
#4446 = AXIS2_PLACEMENT_3D ( 'NONE', #4594, #7096, #625 ) ;
#4447 = EDGE_CURVE ( 'NONE', #10107, #2739, #1099, .T. ) ;
#4448 = LINE ( 'NONE', #4497, #4746 ) ;
#4449 = CIRCLE ( 'NONE', #2915, 7.999999999999994671 ) ;
#4450 = VERTEX_POINT ( 'NONE', #2744 ) ;
#4451 = ORIENTED_EDGE ( 'NONE', *, *, #6760, .T. ) ;
#4452 = CARTESIAN_POINT ( 'NONE',  ( -16.26850689640809833, 140.5696653505793563, 10.90000000000000036 ) ) ;
#4453 = CIRCLE ( 'NONE', #8679, 4.000000000000000000 ) ;
#4454 = ORIENTED_EDGE ( 'NONE', *, *, #3096, .F. ) ;
#4455 = CARTESIAN_POINT ( 'NONE',  ( -30.29350689640809335, 112.5696653505793705, 20.00000000000000711 ) ) ;
#4456 = CARTESIAN_POINT ( 'NONE',  ( -7.293506896408097795, 150.5696653505793563, -20.00000000000000711 ) ) ;
#4457 = CARTESIAN_POINT ( 'NONE',  ( -30.29350689640809335, 128.5696653505793847, 20.00000000000000711 ) ) ;
#4458 = DIRECTION ( 'NONE',  ( -1.000000000000000000, 0.000000000000000000, -0.000000000000000000 ) ) ;
#4459 = ORIENTED_EDGE ( 'NONE', *, *, #789, .T. ) ;
#4460 = VECTOR ( 'NONE', #5563, 1000.000000000000000 ) ;
#4461 = EDGE_LOOP ( 'NONE', ( #5273, #809 ) ) ;
#4462 = EDGE_CURVE ( 'NONE', #6373, #1903, #6497, .T. ) ;
#4463 = EDGE_CURVE ( 'NONE', #8767, #2192, #10063, .T. ) ;
#4464 = VERTEX_POINT ( 'NONE', #1896 ) ;
#4465 = ORIENTED_EDGE ( 'NONE', *, *, #8865, .F. ) ;
#4466 = LINE ( 'NONE', #7754, #8936 ) ;
#4467 = DIRECTION ( 'NONE',  ( 0.000000000000000000, -1.000000000000000000, -1.431206729101514631E-16 ) ) ;
#4468 = VECTOR ( 'NONE', #2850, 1000.000000000000114 ) ;
#4469 = DIRECTION ( 'NONE',  ( 0.000000000000000000, -1.000000000000000000, -9.100899318238123202E-17 ) ) ;
#4470 = CARTESIAN_POINT ( 'NONE',  ( -2.293506896408097795, 80.56966535057935630, -20.00000000000000711 ) ) ;
#4471 = PRODUCT_DEFINITION_FORMATION_WITH_SPECIFIED_SOURCE ( 'ANY', '', #8815, .NOT_KNOWN. ) ;
#4472 = CARTESIAN_POINT ( 'NONE',  ( 23.15769640663940265, -135.1457019118818721, -48.00000000000002132 ) ) ;
#4473 = EDGE_LOOP ( 'NONE', ( #7603, #4700 ) ) ;
#4474 = CARTESIAN_POINT ( 'NONE',  ( -2.293506896408097795, 120.5696653505793705, 20.00000000000000711 ) ) ;
#4475 = AXIS2_PLACEMENT_3D ( 'NONE', #9689, #3213, #9906 ) ;
#4476 = DIRECTION ( 'NONE',  ( -1.000000000000000000, 0.000000000000000000, -8.379529552680125332E-16 ) ) ;
#4477 = CARTESIAN_POINT ( 'NONE',  ( 23.15769640663940265, -133.1457019118818721, -48.00000000000002132 ) ) ;
#4478 = CIRCLE ( 'NONE', #750, 10.00000000000000000 ) ;
#4479 = CARTESIAN_POINT ( 'NONE',  ( 0.000000000000000000, -135.1457019118818721, 49.99999999999997868 ) ) ;
#4480 = CYLINDRICAL_SURFACE ( 'NONE', #3284, 2.000000000000001776 ) ;
#4481 = CARTESIAN_POINT ( 'NONE',  ( -40.00000000000001421, -135.1457019118818721, -40.00000000000002132 ) ) ;
#4482 = DIRECTION ( 'NONE',  ( -0.08084652178105136699, -0.9929337167712568579, -0.08687044385015690873 ) ) ;
#4483 = ORIENTED_EDGE ( 'NONE', *, *, #7033, .F. ) ;
#4484 = CARTESIAN_POINT ( 'NONE',  ( -27.85255513972543895, 64.37996872128307757, 7.750000000000002665 ) ) ;
#4485 = ORIENTED_EDGE ( 'NONE', *, *, #3788, .F. ) ;
#4486 = EDGE_LOOP ( 'NONE', ( #1155, #6410, #7621, #8203 ) ) ;
#4487 = CARTESIAN_POINT ( 'NONE',  ( -16.29350689640809691, 65.65569765742554864, 0.000000000000000000 ) ) ;
#4488 = ADVANCED_FACE ( 'NONE', ( #3652, #9217 ), #1265, .F. ) ;
#4489 = ORIENTED_EDGE ( 'NONE', *, *, #1683, .F. ) ;
#4490 = ORIENTED_EDGE ( 'NONE', *, *, #2882, .T. ) ;
#4491 = DIRECTION ( 'NONE',  ( 1.000000000000000000, -0.000000000000000000, -0.000000000000000000 ) ) ;
#4492 = CARTESIAN_POINT ( 'NONE',  ( -31.74999999999995737, 0.000000000000000000, 0.000000000000000000 ) ) ;
#4493 = ORIENTED_EDGE ( 'NONE', *, *, #1904, .F. ) ;
#4494 = CARTESIAN_POINT ( 'NONE',  ( 39.99999999999997158, -135.1457019118818721, 35.97499999999998010 ) ) ;
#4495 = CARTESIAN_POINT ( 'NONE',  ( 3.000000000000000000, -2.935248768560057009, 4.770489558936219510E-15 ) ) ;
#4496 = CARTESIAN_POINT ( 'NONE',  ( -148.1113867028520872, 243.0027477556404563, 0.000000000000000000 ) ) ;
#4497 = CARTESIAN_POINT ( 'NONE',  ( 25.15769640663940265, -115.1457019118818863, -48.00000000000002132 ) ) ;
#4498 = ORIENTED_EDGE ( 'NONE', *, *, #3642, .T. ) ;
#4499 = EDGE_LOOP ( 'NONE', ( #9434, #6351, #1186 ) ) ;
#4500 = DIRECTION ( 'NONE',  ( -0.6691306063588562392, -0.7431448254773959095, 0.000000000000000000 ) ) ;
#4501 = EDGE_CURVE ( 'NONE', #13, #2946, #6829, .T. ) ;
#4502 = ADVANCED_FACE ( 'NONE', ( #1318 ), #7575, .F. ) ;
#4503 = AXIS2_PLACEMENT_3D ( 'NONE', #10274, #5491, #1474 ) ;
#4504 = EDGE_CURVE ( 'NONE', #2069, #8, #437, .T. ) ;
#4505 = ORIENTED_EDGE ( 'NONE', *, *, #7658, .F. ) ;
#4506 = DIRECTION ( 'NONE',  ( 1.000000000000000000, 0.000000000000000000, 0.000000000000000000 ) ) ;
#4507 = FACE_OUTER_BOUND ( 'NONE', #9738, .T. ) ;
#4508 = CIRCLE ( 'NONE', #9418, 2.445500000000000007 ) ;
#4509 = DIRECTION ( 'NONE',  ( -0.7431448254773957984, 0.6691306063588565722, -0.000000000000000000 ) ) ;
#4510 = DIRECTION ( 'NONE',  ( 0.000000000000000000, 0.5735764363510471586, 0.8191520442889911324 ) ) ;
#4511 = CARTESIAN_POINT ( 'NONE',  ( -38.96131932220313132, 3.319229491889295502, -2.232199717805805061 ) ) ;
#4512 = ORIENTED_EDGE ( 'NONE', *, *, #4109, .T. ) ;
#4513 = CIRCLE ( 'NONE', #292, 7.725331121244574994 ) ;
#4514 = EDGE_LOOP ( 'NONE', ( #3696, #10054, #9519, #7299 ) ) ;
#4515 = ORIENTED_EDGE ( 'NONE', *, *, #9181, .T. ) ;
#4516 = EDGE_CURVE ( 'NONE', #5311, #910, #2797, .T. ) ;
#4517 = VERTEX_POINT ( 'NONE', #8419 ) ;
#4518 = DIRECTION ( 'NONE',  ( 0.000000000000000000, 0.000000000000000000, 1.000000000000000000 ) ) ;
#4519 = DIRECTION ( 'NONE',  ( 0.000000000000000000, 0.000000000000000000, 1.000000000000000000 ) ) ;
#4520 = AXIS2_PLACEMENT_3D ( 'NONE', #9150, #3431, #1890 ) ;
#4521 = LINE ( 'NONE', #2874, #6544 ) ;
#4522 = DIRECTION ( 'NONE',  ( -0.7431448254773957984, 0.6691306063588565722, -0.000000000000000000 ) ) ;
#4523 = PRESENTATION_LAYER_ASSIGNMENT (  '', '', ( #3509 ) ) ;
#4524 = DIRECTION ( 'NONE',  ( -0.000000000000000000, 1.000000000000000000, -0.000000000000000000 ) ) ;
#4525 = VERTEX_POINT ( 'NONE', #9324 ) ;
#4526 = CARTESIAN_POINT ( 'NONE',  ( -40.33539666817953417, 3.509733943237267617, -1.920962489263991158 ) ) ;
#4527 = VECTOR ( 'NONE', #3246, 1000.000000000000000 ) ;
#4528 = DIRECTION ( 'NONE',  ( -0.000000000000000000, -1.000000000000000000, -0.000000000000000000 ) ) ;
#4529 = CIRCLE ( 'NONE', #10458, 4.000000000000000000 ) ;
#4530 = ORIENTED_EDGE ( 'NONE', *, *, #8937, .F. ) ;
#4531 = VECTOR ( 'NONE', #9770, 1000.000000000000000 ) ;
#4532 = CARTESIAN_POINT ( 'NONE',  ( -39.94539818030332157, 129.0132282531173757, 3.999999999999988898 ) ) ;
#4533 = CYLINDRICAL_SURFACE ( 'NONE', #4303, 7.525240063345735919 ) ;
#4534 = ADVANCED_FACE ( 'NONE', ( #1160 ), #4322, .F. ) ;
#4535 = DIRECTION ( 'NONE',  ( 0.000000000000000000, 0.000000000000000000, -1.000000000000000000 ) ) ;
#4536 = VERTEX_POINT ( 'NONE', #10066 ) ;
#4537 = CYLINDRICAL_SURFACE ( 'NONE', #9696, 10.00000000000000178 ) ;
#4538 = ORIENTED_EDGE ( 'NONE', *, *, #3313, .T. ) ;
#4539 = ORIENTED_EDGE ( 'NONE', *, *, #7165, .F. ) ;
#4540 = AXIS2_PLACEMENT_3D ( 'NONE', #8476, #1111, #5137 ) ;
#4541 = LINE ( 'NONE', #9419, #121 ) ;
#4542 = VERTEX_POINT ( 'NONE', #4496 ) ;
#4543 = EDGE_LOOP ( 'NONE', ( #9341, #1866 ) ) ;
#4544 = DIRECTION ( 'NONE',  ( 0.000000000000000000, 0.000000000000000000, 1.000000000000000000 ) ) ;
#4545 = CARTESIAN_POINT ( 'NONE',  ( -155.4728935706336301, 261.2517229562222951, 0.000000000000000000 ) ) ;
#4546 = PRESENTATION_STYLE_ASSIGNMENT (( #7147 ) ) ;
#4547 = DIRECTION ( 'NONE',  ( 0.000000000000000000, 0.000000000000000000, 1.000000000000000000 ) ) ;
#4548 = CARTESIAN_POINT ( 'NONE',  ( -30.29350689640809335, 150.5696653505793563, 0.000000000000000000 ) ) ;
#4549 = CIRCLE ( 'NONE', #8270, 26.75575292317714116 ) ;
#4550 = CARTESIAN_POINT ( 'NONE',  ( -40.33539666817950575, -3.509733943237241416, -1.920962489264039785 ) ) ;
#4551 = EDGE_CURVE ( 'NONE', #1811, #8738, #2631, .T. ) ;
#4552 = AXIS2_PLACEMENT_3D ( 'NONE', #4319, #8189, #1085 ) ;
#4553 = ORIENTED_EDGE ( 'NONE', *, *, #4310, .F. ) ;
#4554 = CARTESIAN_POINT ( 'NONE',  ( -56.36957570605427037, 137.0132282531173473, 0.000000000000000000 ) ) ;
#4555 = ORIENTED_EDGE ( 'NONE', *, *, #789, .F. ) ;
#4556 = CARTESIAN_POINT ( 'NONE',  ( -50.00000000000002842, -135.1457019118818721, 26.62179802177713484 ) ) ;
#4557 = CIRCLE ( 'NONE', #4399, 3.999999999999999112 ) ;
#4558 = DIRECTION ( 'NONE',  ( -0.7431448254773957984, 0.6691306063588565722, -0.000000000000000000 ) ) ;
#4559 = CARTESIAN_POINT ( 'NONE',  ( -8.000000000000000000, -1.871412446612475522, 0.8726539554219646666 ) ) ;
#4560 = PLANE ( 'NONE',  #1597 ) ;
#4561 = ORIENTED_EDGE ( 'NONE', *, *, #5641, .T. ) ;
#4562 = ADVANCED_FACE ( 'NONE', ( #7149 ), #4597, .F. ) ;
#4563 = ADVANCED_FACE ( 'NONE', ( #6395 ), #3965, .F. ) ;
#4564 = ADVANCED_FACE ( 'NONE', ( #7248 ), #5598, .F. ) ;
#4565 = VERTEX_POINT ( 'NONE', #8034 ) ;
#4566 =( REPRESENTATION_RELATIONSHIP ('NONE','NONE', #9007, #5068 ) REPRESENTATION_RELATIONSHIP_WITH_TRANSFORMATION ( #1721 )SHAPE_REPRESENTATION_RELATIONSHIP( ) );
#4567 = VERTEX_POINT ( 'NONE', #2324 ) ;
#4568 = ORIENTED_EDGE ( 'NONE', *, *, #8109, .T. ) ;
#4569 = FACE_OUTER_BOUND ( 'NONE', #7092, .T. ) ;
#4570 = DIRECTION ( 'NONE',  ( -1.396588258780021135E-16, -0.000000000000000000, 1.000000000000000000 ) ) ;
#4571 = CARTESIAN_POINT ( 'NONE',  ( 14.70649310359190309, 120.5696653505793705, 24.00000000000000711 ) ) ;
#4572 = FACE_OUTER_BOUND ( 'NONE', #8518, .T. ) ;
#4573 = DIRECTION ( 'NONE',  ( 1.000000000000000000, 0.000000000000000000, 0.000000000000000000 ) ) ;
#4574 = ADVANCED_FACE ( 'NONE', ( #681 ), #1107, .F. ) ;
#4575 = ORIENTED_EDGE ( 'NONE', *, *, #10218, .F. ) ;
#4576 = CARTESIAN_POINT ( 'NONE',  ( -67.94539818030330025, 155.5289575273812090, 0.000000000000000000 ) ) ;
#4577 = CARTESIAN_POINT ( 'NONE',  ( -16.29350689640809691, 65.65569765742554864, 0.000000000000000000 ) ) ;
#4578 = DIRECTION ( 'NONE',  ( 0.000000000000000000, -0.9374252720097652203, -0.3481865296036273372 ) ) ;
#4579 = DIRECTION ( 'NONE',  ( -1.000000000000000000, 0.000000000000000000, 0.000000000000000000 ) ) ;
#4580 = DIRECTION ( 'NONE',  ( -0.6585271261848805180, 0.7525569905852198538, 0.000000000000000000 ) ) ;
#4581 = PLANE ( 'NONE',  #4828 ) ;
#4582 = ORIENTED_EDGE ( 'NONE', *, *, #7423, .T. ) ;
#4583 = VECTOR ( 'NONE', #2420, 1000.000000000000000 ) ;
#4584 = FACE_OUTER_BOUND ( 'NONE', #4280, .T. ) ;
#4585 = VERTEX_POINT ( 'NONE', #7045 ) ;
#4586 = PRODUCT_CONTEXT ( 'NONE', #8219, 'mechanical' ) ;
#4587 = VERTEX_POINT ( 'NONE', #1370 ) ;
#4588 = CARTESIAN_POINT ( 'NONE',  ( 42.22511195853866184, 52.77167129626698028, -30.00000000000000355 ) ) ;
#4589 = ORIENTED_EDGE ( 'NONE', *, *, #4252, .T. ) ;
#4590 = ADVANCED_FACE ( 'NONE', ( #5495 ), #10281, .F. ) ;
#4591 = CIRCLE ( 'NONE', #8150, 2.999999999999999556 ) ;
#4592 = ORIENTED_EDGE ( 'NONE', *, *, #6735, .F. ) ;
#4593 = CYLINDRICAL_SURFACE ( 'NONE', #4503, 2.000000000000001776 ) ;
#4594 = CARTESIAN_POINT ( 'NONE',  ( -16.29350689640809691, -8.660287962196477451, 0.000000000000000000 ) ) ;
#4595 = ORIENTED_EDGE ( 'NONE', *, *, #4179, .F. ) ;
#4596 = CARTESIAN_POINT ( 'NONE',  ( -149.7944168144651655, 241.1335534508485807, 0.000000000000000000 ) ) ;
#4597 = CYLINDRICAL_SURFACE ( 'NONE', #8726, 2.000000000000001776 ) ;
#4598 = DIRECTION ( 'NONE',  ( 0.000000000000000000, -1.000000000000000000, 0.000000000000000000 ) ) ;
#4599 = CARTESIAN_POINT ( 'NONE',  ( -141.4979315611417690, 196.0297649204779589, -4.790608351577442020E-15 ) ) ;
#4600 = CIRCLE ( 'NONE', #2566, 4.999999999999997335 ) ;
#4601 = AXIS2_PLACEMENT_3D ( 'NONE', #8586, #5983, #5928 ) ;
#4602 = ORIENTED_EDGE ( 'NONE', *, *, #4108, .T. ) ;
#4603 = FACE_BOUND ( 'NONE', #8083, .T. ) ;
#4604 = ORIENTED_EDGE ( 'NONE', *, *, #1199, .T. ) ;
#4605 = EDGE_CURVE ( 'NONE', #1455, #2553, #4797, .T. ) ;
#4606 = DIRECTION ( 'NONE',  ( -0.6691306063588562392, -0.7431448254773960205, 0.000000000000000000 ) ) ;
#4607 = PLANE ( 'NONE',  #4927 ) ;
#4608 = ORIENTED_EDGE ( 'NONE', *, *, #1594, .F. ) ;
#4609 = VECTOR ( 'NONE', #9583, 1000.000000000000000 ) ;
#4610 = CARTESIAN_POINT ( 'NONE',  ( 27.15769640663936713, -133.1457019118818721, 27.15769640663938489 ) ) ;
#4611 = CARTESIAN_POINT ( 'NONE',  ( -47.94539818030328604, 155.5289575273811522, -4.000000000000000000 ) ) ;
#4612 = CYLINDRICAL_SURFACE ( 'NONE', #7703, 4.000000000000000000 ) ;
#4613 = VERTEX_POINT ( 'NONE', #9648 ) ;
#4614 = ORIENTED_EDGE ( 'NONE', *, *, #10327, .T. ) ;
#4615 = VECTOR ( 'NONE', #5524, 1000.000000000000000 ) ;
#4616 = ORIENTED_EDGE ( 'NONE', *, *, #2521, .T. ) ;
#4617 = VERTEX_POINT ( 'NONE', #6347 ) ;
#4618 = EDGE_CURVE ( 'NONE', #2709, #1613, #10380, .T. ) ;
#4619 = CARTESIAN_POINT ( 'NONE',  ( 37.59878849545336976, 32.08684478514406635, 30.00000000000000355 ) ) ;
#4620 = CARTESIAN_POINT ( 'NONE',  ( -47.94539818030330025, 90.52895752738122326, -3.999999999999993339 ) ) ;
#4621 = ADVANCED_FACE ( 'NONE', ( #10334 ), #727, .T. ) ;
#4622 = DIRECTION ( 'NONE',  ( 0.000000000000000000, 1.000000000000000000, -0.000000000000000000 ) ) ;
#4623 = CARTESIAN_POINT ( 'NONE',  ( -2.293506896408097795, 80.56966535057935630, 20.00000000000000711 ) ) ;
#4624 = CIRCLE ( 'NONE', #61, 4.000000000000000000 ) ;
#4625 = LINE ( 'NONE', #9827, #8226 ) ;
#4626 = EDGE_LOOP ( 'NONE', ( #4949, #9246, #4230, #8173 ) ) ;
#4627 = DIRECTION ( 'NONE',  ( -1.000000000000000000, -0.000000000000000000, -0.000000000000000000 ) ) ;
#4628 = APPLICATION_CONTEXT ( 'automotive_design' ) ;
#4629 = AXIS2_PLACEMENT_3D ( 'NONE', #1848, #6614, #5817 ) ;
#4630 = ORIENTED_EDGE ( 'NONE', *, *, #3540, .F. ) ;
#4631 = EDGE_CURVE ( 'NONE', #5630, #9939, #5501, .T. ) ;
#4632 = FACE_BOUND ( 'NONE', #4858, .T. ) ;
#4633 = ADVANCED_FACE ( 'NONE', ( #2215 ), #5444, .T. ) ;
#4634 = CONICAL_SURFACE ( 'NONE', #8032, 2.541999999999999815, 1.047197551196591858 ) ;
#4635 = EDGE_CURVE ( 'NONE', #9925, #6753, #10417, .T. ) ;
#4636 = CARTESIAN_POINT ( 'NONE',  ( -39.00000000000000000, -3.117691453623975484, -1.800000000000017586 ) ) ;
#4637 = LINE ( 'NONE', #1462, #3127 ) ;
#4638 = VECTOR ( 'NONE', #8677, 1000.000000000000000 ) ;
#4639 = ORIENTED_EDGE ( 'NONE', *, *, #1627, .F. ) ;
#4640 = DIRECTION ( 'NONE',  ( 1.000000000000000000, 1.277197683604454965E-16, -0.000000000000000000 ) ) ;
#4641 = AXIS2_PLACEMENT_3D ( 'NONE', #10008, #5965, #9206 ) ;
#4642 = CARTESIAN_POINT ( 'NONE',  ( -36.29350689640810401, 80.56966535057935630, 19.99999999999996092 ) ) ;
#4643 = ORIENTED_EDGE ( 'NONE', *, *, #303, .T. ) ;
#4644 = FACE_OUTER_BOUND ( 'NONE', #854, .T. ) ;
#4645 = ORIENTED_EDGE ( 'NONE', *, *, #5347, .T. ) ;
#4646 = EDGE_CURVE ( 'NONE', #8095, #5671, #5834, .T. ) ;
#4647 = ORIENTED_EDGE ( 'NONE', *, *, #4331, .F. ) ;
#4648 = CARTESIAN_POINT ( 'NONE',  ( -158.9246696254695337, 264.3597160760069187, 0.000000000000000000 ) ) ;
#4649 = DIRECTION ( 'NONE',  ( -0.000000000000000000, -0.000000000000000000, -1.000000000000000000 ) ) ;
#4650 = CARTESIAN_POINT ( 'NONE',  ( -24.31850689640809549, 140.5696653505793563, 10.90000000000000036 ) ) ;
#4651 = DIRECTION ( 'NONE',  ( 0.000000000000000000, 0.000000000000000000, -1.000000000000000000 ) ) ;
#4652 = DIRECTION ( 'NONE',  ( -8.194486552889013533E-17, -9.100899318238110877E-17, 1.000000000000000000 ) ) ;
#4653 = CARTESIAN_POINT ( 'NONE',  ( 53.40242741783141156, 52.77167129626698028, 25.00000000000000000 ) ) ;
#4654 = CARTESIAN_POINT ( 'NONE',  ( 39.99999999999997158, -145.1457019118819005, 39.99999999999997868 ) ) ;
#4655 = EDGE_CURVE ( 'NONE', #640, #5617, #7536, .T. ) ;
#4656 = AXIS2_PLACEMENT_3D ( 'NONE', #3128, #1494, #1543 ) ;
#4657 = EDGE_LOOP ( 'NONE', ( #4553, #3084, #2950, #6461 ) ) ;
#4658 = DIRECTION ( 'NONE',  ( 0.000000000000000000, 0.000000000000000000, 1.000000000000000000 ) ) ;
#4659 = VECTOR ( 'NONE', #2335, 1000.000000000000000 ) ;
#4660 = EDGE_LOOP ( 'NONE', ( #1829, #9369, #7787, #2122 ) ) ;
#4661 = LINE ( 'NONE', #9809, #1328 ) ;
#4662 = LINE ( 'NONE', #689, #2237 ) ;
#4663 = DIRECTION ( 'NONE',  ( 0.000000000000000000, 0.000000000000000000, -1.000000000000000000 ) ) ;
#4664 = CYLINDRICAL_SURFACE ( 'NONE', #8768, 5.000000000000004441 ) ;
#4665 = AXIS2_PLACEMENT_3D ( 'NONE', #372, #3600, #5284 ) ;
#4666 = CARTESIAN_POINT ( 'NONE',  ( -20.29350689640809691, 140.5696653505793563, 7.750000000000001776 ) ) ;
#4667 = ORIENTED_EDGE ( 'NONE', *, *, #9826, .T. ) ;
#4668 = EDGE_CURVE ( 'NONE', #9380, #9915, #3163, .T. ) ;
#4669 = ORIENTED_EDGE ( 'NONE', *, *, #8123, .T. ) ;
#4670 = VECTOR ( 'NONE', #9838, 1000.000000000000000 ) ;
#4671 = VECTOR ( 'NONE', #1678, 1000.000000000000114 ) ;
#4672 = ORIENTED_EDGE ( 'NONE', *, *, #1932, .T. ) ;
#4673 = ORIENTED_EDGE ( 'NONE', *, *, #2170, .F. ) ;
#4674 =( BOUNDED_CURVE ( )  B_SPLINE_CURVE ( 3, ( #4170, #4853, #8090, #3427 ),
 .UNSPECIFIED., .F., .T. ) 
 B_SPLINE_CURVE_WITH_KNOTS ( ( 4, 4 ),
 ( 1.570796326794896558, 3.141592653589795781 ),
 .UNSPECIFIED. ) 
 CURVE ( )  GEOMETRIC_REPRESENTATION_ITEM ( )  RATIONAL_B_SPLINE_CURVE ( ( 1.000000000000000000, 0.8047378541243643824, 0.8047378541243643824, 1.000000000000000000 ) ) 
 REPRESENTATION_ITEM ( '' )  );
#4675 = DIRECTION ( 'NONE',  ( -1.277197683604454965E-16, 1.000000000000000000, 0.000000000000000000 ) ) ;
#4676 = CARTESIAN_POINT ( 'NONE',  ( 0.000000000000000000, 55.56966535057937051, 0.000000000000000000 ) ) ;
#4677 = DIRECTION ( 'NONE',  ( -1.000000000000000000, -0.000000000000000000, -0.000000000000000000 ) ) ;
#4678 = DIRECTION ( 'NONE',  ( 1.000000000000000000, -0.000000000000000000, -0.000000000000000000 ) ) ;
#4679 = CONICAL_SURFACE ( 'NONE', #5186, 2.445500000000000007, 0.7853981633974547183 ) ;
#4680 = FACE_OUTER_BOUND ( 'NONE', #10394, .T. ) ;
#4681 = CIRCLE ( 'NONE', #5852, 7.794205612481196255 ) ;
#4682 = EDGE_LOOP ( 'NONE', ( #3571, #5451, #72, #438 ) ) ;
#4683 = DIRECTION ( 'NONE',  ( -1.000000000000000000, -0.000000000000000000, -0.000000000000000000 ) ) ;
#4684 = ADVANCED_FACE ( 'NONE', ( #7986 ), #8297, .F. ) ;
#4685 = VECTOR ( 'NONE', #2640, 1000.000000000000000 ) ;
#4686 = EDGE_LOOP ( 'NONE', ( #6123, #4604, #4489, #3142 ) ) ;
#4687 = CARTESIAN_POINT ( 'NONE',  ( -39.65624476065125492, 3.117691453623999909, -1.799999999999972955 ) ) ;
#4688 = VECTOR ( 'NONE', #7026, 1000.000000000000000 ) ;
#4689 = CARTESIAN_POINT ( 'NONE',  ( 49.99999999999998579, -145.1457019118819005, -40.00000000000002132 ) ) ;
#4690 = DIRECTION ( 'NONE',  ( 7.848480207562752404E-17, 1.000000000000000000, -7.143558635763577733E-33 ) ) ;
#4691 = CARTESIAN_POINT ( 'NONE',  ( 37.22511195853868315, -116.6161171811496331, 25.10513196898123311 ) ) ;
#4692 = AXIS2_PLACEMENT_3D ( 'NONE', #9940, #9886, #1763 ) ;
#4693 = ORIENTED_EDGE ( 'NONE', *, *, #5458, .T. ) ;
#4694 = ADVANCED_FACE ( 'NONE', ( #94 ), #3377, .T. ) ;
#4695 = ADVANCED_FACE ( 'NONE', ( #151 ), #4223, .F. ) ;
#4696 = EDGE_CURVE ( 'NONE', #1043, #195, #9922, .T. ) ;
#4697 = AXIS2_PLACEMENT_3D ( 'NONE', #6950, #6093, #3666 ) ;
#4698 = ORIENTED_EDGE ( 'NONE', *, *, #8630, .T. ) ;
#4699 = DIRECTION ( 'NONE',  ( 0.000000000000000000, 0.000000000000000000, 1.000000000000000000 ) ) ;
#4700 = ORIENTED_EDGE ( 'NONE', *, *, #4050, .T. ) ;
#4701 = AXIS2_PLACEMENT_3D ( 'NONE', #7332, #77, #3301 ) ;
#4702 = CARTESIAN_POINT ( 'NONE',  ( -2.293506896408097795, 55.56966535057937051, 0.000000000000000000 ) ) ;
#4703 = CARTESIAN_POINT ( 'NONE',  ( 2.275687196221498316E-14, -133.1457019118818721, -27.15769640663941686 ) ) ;
#4704 = DIRECTION ( 'NONE',  ( 0.000000000000000000, 0.000000000000000000, 1.000000000000000000 ) ) ;
#4705 = DIRECTION ( 'NONE',  ( 0.000000000000000000, -1.000000000000000000, 0.000000000000000000 ) ) ;
#4706 = DIRECTION ( 'NONE',  ( -0.000000000000000000, -0.000000000000000000, -1.000000000000000000 ) ) ;
#4707 = DIRECTION ( 'NONE',  ( 1.000000000000000000, -0.000000000000000000, -0.000000000000000000 ) ) ;
#4708 = CIRCLE ( 'NONE', #5373, 4.000000000000000000 ) ;
#4709 = EDGE_CURVE ( 'NONE', #8369, #5250, #271, .T. ) ;
#4710 = EDGE_CURVE ( 'NONE', #847, #4386, #1113, .T. ) ;
#4711 = ORIENTED_EDGE ( 'NONE', *, *, #4215, .F. ) ;
#4712 = FACE_OUTER_BOUND ( 'NONE', #2919, .T. ) ;
#4713 = AXIS2_PLACEMENT_3D ( 'NONE', #6339, #4791, #9684 ) ;
#4714 = ORIENTED_EDGE ( 'NONE', *, *, #4154, .T. ) ;
#4715 = CARTESIAN_POINT ( 'NONE',  ( 23.15769640663936713, -133.1457019118818721, 47.99999999999997868 ) ) ;
#4716 = DIRECTION ( 'NONE',  ( -1.000000000000000000, 0.000000000000000000, 0.000000000000000000 ) ) ;
#4717 = CIRCLE ( 'NONE', #154, 4.024999999999997691 ) ;
#4718 = DIRECTION ( 'NONE',  ( 0.000000000000000000, 1.000000000000000000, -1.329743448921561232E-15 ) ) ;
#4719 = DIRECTION ( 'NONE',  ( -1.000000000000000000, -0.000000000000000000, -0.000000000000000000 ) ) ;
#4720 = ORIENTED_EDGE ( 'NONE', *, *, #6789, .F. ) ;
#4721 = ORIENTED_EDGE ( 'NONE', *, *, #6494, .F. ) ;
#4722 = VERTEX_POINT ( 'NONE', #6442 ) ;
#4723 = DIRECTION ( 'NONE',  ( 0.000000000000000000, 0.000000000000000000, 1.000000000000000000 ) ) ;
#4724 = EDGE_CURVE ( 'NONE', #581, #3561, #3483, .T. ) ;
#4725 = CARTESIAN_POINT ( 'NONE',  ( -47.94539818030330025, 150.5696653505793563, 0.000000000000000000 ) ) ;
#4726 = FACE_OUTER_BOUND ( 'NONE', #675, .T. ) ;
#4727 = CYLINDRICAL_SURFACE ( 'NONE', #5463, 3.999999999999989786 ) ;
#4728 = CARTESIAN_POINT ( 'NONE',  ( -27.15769640663939555, -133.1457019118818721, -27.15769640663944173 ) ) ;
#4729 = ORIENTED_EDGE ( 'NONE', *, *, #9294, .T. ) ;
#4730 = DIRECTION ( 'NONE',  ( -0.000000000000000000, -0.000000000000000000, -1.000000000000000000 ) ) ;
#4731 = ORIENTED_EDGE ( 'NONE', *, *, #6433, .F. ) ;
#4732 = CARTESIAN_POINT ( 'NONE',  ( -48.00000000000002132, -135.1457019118818721, 27.15769640663938489 ) ) ;
#4733 = EDGE_CURVE ( 'NONE', #10120, #9924, #4272, .T. ) ;
#4734 = CARTESIAN_POINT ( 'NONE',  ( 23.15769640663940265, -133.1457019118818721, -50.00000000000002132 ) ) ;
#4735 = CYLINDRICAL_SURFACE ( 'NONE', #7210, 4.999999999999997335 ) ;
#4736 = ORIENTED_EDGE ( 'NONE', *, *, #2873, .T. ) ;
#4737 = CARTESIAN_POINT ( 'NONE',  ( -48.00000000000002132, -133.1457019118818721, -23.15769640663945594 ) ) ;
#4738 = ORIENTED_EDGE ( 'NONE', *, *, #9049, .T. ) ;
#4739 = DIRECTION ( 'NONE',  ( -0.7431448254773957984, 0.6691306063588565722, -0.000000000000000000 ) ) ;
#4740 = EDGE_LOOP ( 'NONE', ( #1593, #2485, #2897, #5436 ) ) ;
#4741 = DIRECTION ( 'NONE',  ( 1.000000000000000000, 0.000000000000000000, 0.000000000000000000 ) ) ;
#4742 = EDGE_CURVE ( 'NONE', #2698, #9534, #5007, .T. ) ;
#4743 = ADVANCED_FACE ( 'NONE', ( #6658 ), #3315, .F. ) ;
#4744 = EDGE_CURVE ( 'NONE', #1800, #7344, #5855, .T. ) ;
#4745 = CARTESIAN_POINT ( 'NONE',  ( 14.70649310359190309, 80.56966535057935630, 20.00000000000000711 ) ) ;
#4746 = VECTOR ( 'NONE', #9378, 1000.000000000000000 ) ;
#4747 = DIRECTION ( 'NONE',  ( 0.6585271261848814062, -0.7525569905852189656, -6.854174792162727679E-16 ) ) ;
#4748 = CARTESIAN_POINT ( 'NONE',  ( -16.29350689640809691, 88.12362273389504708, 4.729641367753004033 ) ) ;
#4749 = SPHERICAL_SURFACE ( 'NONE', #3067, 2.000000000000000000 ) ;
#4750 = FACE_OUTER_BOUND ( 'NONE', #10193, .T. ) ;
#4751 = ORIENTED_EDGE ( 'NONE', *, *, #10279, .T. ) ;
#4752 = CARTESIAN_POINT ( 'NONE',  ( 59.99999999999999289, -145.1457019118819005, -30.00000000000000355 ) ) ;
#4753 = ORIENTED_EDGE ( 'NONE', *, *, #1110, .F. ) ;
#4754 = DIRECTION ( 'NONE',  ( -0.000000000000000000, 1.000000000000000000, 0.000000000000000000 ) ) ;
#4755 = DIRECTION ( 'NONE',  ( -0.000000000000000000, 1.000000000000000000, -0.000000000000000000 ) ) ;
#4756 = ADVANCED_FACE ( 'NONE', ( #4117 ), #9096, .F. ) ;
#4757 = ADVANCED_FACE ( 'NONE', ( #1036 ), #8940, .F. ) ;
#4758 = VERTEX_POINT ( 'NONE', #9692 ) ;
#4759 = PLANE ( 'NONE',  #564 ) ;
#4760 = CARTESIAN_POINT ( 'NONE',  ( -21.29350689640810046, 105.5289575273812233, 10.90000000000000036 ) ) ;
#4761 = AXIS2_PLACEMENT_3D ( 'NONE', #10344, #4716, #737 ) ;
#4762 = DIRECTION ( 'NONE',  ( 0.000000000000000000, 0.000000000000000000, 1.000000000000000000 ) ) ;
#4763 = CIRCLE ( 'NONE', #5613, 4.000000000000003553 ) ;
#4764 = ORIENTED_EDGE ( 'NONE', *, *, #8508, .F. ) ;
#4765 = ORIENTED_EDGE ( 'NONE', *, *, #3182, .F. ) ;
#4766 = CIRCLE ( 'NONE', #8330, 5.000000000000001776 ) ;
#4767 = ORIENTED_EDGE ( 'NONE', *, *, #2654, .F. ) ;
#4768 = AXIS2_PLACEMENT_3D ( 'NONE', #7615, #10161, #3639 ) ;
#4769 = DIRECTION ( 'NONE',  ( 0.000000000000000000, 0.000000000000000000, 1.000000000000000000 ) ) ;
#4770 = DIRECTION ( 'NONE',  ( 0.000000000000000000, -1.000000000000000000, -9.100899318238112109E-17 ) ) ;
#4771 = EDGE_CURVE ( 'NONE', #2451, #10264, #9242, .T. ) ;
#4772 = CARTESIAN_POINT ( 'NONE',  ( -24.41866285951199345, -134.3099192498708874, -50.00000000000002132 ) ) ;
#4773 = CARTESIAN_POINT ( 'NONE',  ( -121.1992630477586346, 230.3916074206559017, 0.000000000000000000 ) ) ;
#4774 = CARTESIAN_POINT ( 'NONE',  ( -121.7299640054770578, 230.8694527092982867, 0.000000000000000000 ) ) ;
#4775 = VECTOR ( 'NONE', #9121, 999.9999999999998863 ) ;
#4776 = VERTEX_POINT ( 'NONE', #42 ) ;
#4777 = AXIS2_PLACEMENT_3D ( 'NONE', #6870, #5225, #7771 ) ;
#4778 = DIRECTION ( 'NONE',  ( 0.000000000000000000, 1.000000000000000000, 0.000000000000000000 ) ) ;
#4779 = EDGE_CURVE ( 'NONE', #7038, #415, #4900, .T. ) ;
#4780 = ORIENTED_EDGE ( 'NONE', *, *, #5334, .F. ) ;
#4781 = ORIENTED_EDGE ( 'NONE', *, *, #7348, .F. ) ;
#4782 = DIRECTION ( 'NONE',  ( -0.000000000000000000, 1.000000000000000000, -0.000000000000000000 ) ) ;
#4783 = VECTOR ( 'NONE', #4195, 1000.000000000000000 ) ;
#4784 = DIRECTION ( 'NONE',  ( 6.982941293900105430E-16, 0.000000000000000000, -1.000000000000000000 ) ) ;
#4785 = CARTESIAN_POINT ( 'NONE',  ( 4.856471286862176662, 145.0444252872335937, 12.50000000000000355 ) ) ;
#4786 = ORIENTED_EDGE ( 'NONE', *, *, #4447, .T. ) ;
#4787 = DIRECTION ( 'NONE',  ( 0.000000000000000000, 0.000000000000000000, 1.000000000000000000 ) ) ;
#4788 = VECTOR ( 'NONE', #8951, 1000.000000000000000 ) ;
#4789 = ITEM_DEFINED_TRANSFORMATION ( 'NONE', 'NONE', #2606,  #4601 ) ;
#4790 = EDGE_LOOP ( 'NONE', ( #8529, #8085, #7990, #3638 ) ) ;
#4791 = DIRECTION ( 'NONE',  ( -1.000000000000000000, -0.000000000000000000, -0.000000000000000000 ) ) ;
#4792 = ORIENTED_EDGE ( 'NONE', *, *, #7994, .F. ) ;
#4793 = VERTEX_POINT ( 'NONE', #9744 ) ;
#4794 = AXIS2_PLACEMENT_3D ( 'NONE', #6657, #5694, #93 ) ;
#4795 = DIRECTION ( 'NONE',  ( 1.000000000000000000, -0.000000000000000000, 8.379529552680125332E-16 ) ) ;
#4796 = LINE ( 'NONE', #3754, #4638 ) ;
#4797 = LINE ( 'NONE', #2960, #6008 ) ;
#4798 = AXIS2_PLACEMENT_3D ( 'NONE', #8526, #422, #5234 ) ;
#4799 = CARTESIAN_POINT ( 'NONE',  ( -30.29350689640809335, 0.000000000000000000, 10.98204862120179826 ) ) ;
#4800 = DIRECTION ( 'NONE',  ( 0.9973063064792990762, 0.07334937666141773394, 0.000000000000000000 ) ) ;
#4801 = EDGE_CURVE ( 'NONE', #5649, #5184, #2468, .T. ) ;
#4802 = ORIENTED_EDGE ( 'NONE', *, *, #3980, .F. ) ;
#4803 = TOROIDAL_SURFACE ( 'NONE', #6163, 11.15107097094592881, 2.515249034521771510 ) ;
#4804 = CARTESIAN_POINT ( 'NONE',  ( -18.34874108452141783, -140.1746510883711778, -24.43989726270230634 ) ) ;
#4805 = ORIENTED_EDGE ( 'NONE', *, *, #9679, .F. ) ;
#4806 = LINE ( 'NONE', #5756, #9115 ) ;
#4807 = CARTESIAN_POINT ( 'NONE',  ( 17.97972049165455388, 37.08684478514405214, 12.50000000000000000 ) ) ;
#4808 = PLANE ( 'NONE',  #5632 ) ;
#4809 = DIRECTION ( 'NONE',  ( 0.000000000000000000, 0.000000000000000000, -1.000000000000000000 ) ) ;
#4810 = AXIS2_PLACEMENT_3D ( 'NONE', #6617, #165, #8954 ) ;
#4811 = DIRECTION ( 'NONE',  ( -0.000000000000000000, 1.000000000000000000, 0.000000000000000000 ) ) ;
#4812 = ORIENTED_EDGE ( 'NONE', *, *, #1709, .F. ) ;
#4813 = ORIENTED_EDGE ( 'NONE', *, *, #9049, .F. ) ;
#4814 = CIRCLE ( 'NONE', #1271, 10.00000000000000178 ) ;
#4815 = ADVANCED_FACE ( 'NONE', ( #8137 ), #7349, .T. ) ;
#4816 = EDGE_CURVE ( 'NONE', #264, #4464, #5514, .T. ) ;
#4817 = EDGE_CURVE ( 'NONE', #3545, #9491, #5321, .T. ) ;
#4818 = EDGE_LOOP ( 'NONE', ( #4925, #3116, #1992, #10022, #4384, #7366, #8181, #5976, #9709, #7827, #4879, #5831, #3158, #4972, #7380, #6621 ) ) ;
#4819 = FACE_BOUND ( 'NONE', #8837, .T. ) ;
#4820 = DIRECTION ( 'NONE',  ( 0.000000000000000000, -0.000000000000000000, 1.000000000000000000 ) ) ;
#4821 = AXIS2_PLACEMENT_3D ( 'NONE', #7730, #473, #8787 ) ;
#4822 = CARTESIAN_POINT ( 'NONE',  ( -27.15769640663940976, -133.1457019118818721, 25.15769640663938134 ) ) ;
#4823 = DIRECTION ( 'NONE',  ( 0.000000000000000000, -0.000000000000000000, 1.000000000000000000 ) ) ;
#4824 = VERTEX_POINT ( 'NONE', #2683 ) ;
#4825 = FACE_OUTER_BOUND ( 'NONE', #5079, .T. ) ;
#4826 = VERTEX_POINT ( 'NONE', #8405 ) ;
#4827 = DIRECTION ( 'NONE',  ( -0.000000000000000000, 1.000000000000000000, -0.000000000000000000 ) ) ;
#4828 = AXIS2_PLACEMENT_3D ( 'NONE', #2144, #612, #10320 ) ;
#4829 = EDGE_CURVE ( 'NONE', #7484, #5250, #9959, .T. ) ;
#4830 = ORIENTED_EDGE ( 'NONE', *, *, #7222, .T. ) ;
#4831 = ORIENTED_EDGE ( 'NONE', *, *, #9472, .F. ) ;
#4832 = FACE_OUTER_BOUND ( 'NONE', #10324, .T. ) ;
#4833 = AXIS2_PLACEMENT_3D ( 'NONE', #2050, #5915, #9155 ) ;
#4834 = CARTESIAN_POINT ( 'NONE',  ( -38.19229777560033057, -43.28483205141633761, -12.50000000000000000 ) ) ;
#4835 = PRODUCT_DEFINITION_SHAPE ( 'NONE', 'NONE',  #10486 ) ;
#4836 = AXIS2_PLACEMENT_3D ( 'NONE', #6056, #9947, #8393 ) ;
#4837 = CARTESIAN_POINT ( 'NONE',  ( -2.293506896408097795, 150.5696653505793563, -20.00000000000000711 ) ) ;
#4838 = CARTESIAN_POINT ( 'NONE',  ( -27.15769640663939199, -135.1457019118818721, -27.15769640663944173 ) ) ;
#4839 = ORIENTED_EDGE ( 'NONE', *, *, #10056, .F. ) ;
#4840 = DIRECTION ( 'NONE',  ( 0.000000000000000000, 0.000000000000000000, -1.000000000000000000 ) ) ;
#4841 = AXIS2_PLACEMENT_3D ( 'NONE', #8440, #6157, #6853 ) ;
#4842 = ORIENTED_EDGE ( 'NONE', *, *, #1643, .F. ) ;
#4843 = DIRECTION ( 'NONE',  ( -7.016001027857739179E-17, -0.8191520442889906883, -0.5735764363510477137 ) ) ;
#4844 = ORIENTED_EDGE ( 'NONE', *, *, #3760, .F. ) ;
#4845 = ORIENTED_EDGE ( 'NONE', *, *, #1124, .T. ) ;
#4846 = ADVANCED_FACE ( 'NONE', ( #1990 ), #2089, .T. ) ;
#4847 = AXIS2_PLACEMENT_3D ( 'NONE', #8413, #10219, #6019 ) ;
#4848 = DIRECTION ( 'NONE',  ( 0.000000000000000000, 0.000000000000000000, -1.000000000000000000 ) ) ;
#4849 = CARTESIAN_POINT ( 'NONE',  ( 3.000000000000000000, 2.935248768560057897, -3.252606517456513302E-15 ) ) ;
#4850 = CARTESIAN_POINT ( 'NONE',  ( -16.29350689640809691, 55.56966535057936341, 0.000000000000000000 ) ) ;
#4851 = CARTESIAN_POINT ( 'NONE',  ( 27.15769640663938489, -133.1457019118818721, -25.15769640663940621 ) ) ;
#4852 = VECTOR ( 'NONE', #2937, 1000.000000000000000 ) ;
#4853 = CARTESIAN_POINT ( 'NONE',  ( 97.72361618343359169, -145.1457019118819005, -30.00000000000000711 ) ) ;
#4854 = ORIENTED_EDGE ( 'NONE', *, *, #7278, .T. ) ;
#4855 = TOROIDAL_SURFACE ( 'NONE', #6220, -16.75790667520975674, 26.17065043502059041 ) ;
#4856 = CARTESIAN_POINT ( 'NONE',  ( -166.5958414309862690, 248.8984378607219980, 0.000000000000000000 ) ) ;
#4857 = AXIS2_PLACEMENT_3D ( 'NONE', #2496, #4244, #8324 ) ;
#4858 = EDGE_LOOP ( 'NONE', ( #7747, #2374 ) ) ;
#4859 = CARTESIAN_POINT ( 'NONE',  ( -7.293506896408097795, 145.5696653505793563, 25.00000000000000711 ) ) ;
#4860 = DIRECTION ( 'NONE',  ( -0.7367503238654704578, 0.6761648913424330720, -0.000000000000000000 ) ) ;
#4861 = CARTESIAN_POINT ( 'NONE',  ( 27.15769640663936713, -117.1457019118819005, 27.15769640663938489 ) ) ;
#4862 = LINE ( 'NONE', #840, #8694 ) ;
#4863 = EDGE_CURVE ( 'NONE', #8078, #2498, #8394, .T. ) ;
#4864 = CARTESIAN_POINT ( 'NONE',  ( 6.000000000000005329, 3.980102097228898231E-16, 3.250000000000000444 ) ) ;
#4865 = AXIS2_PLACEMENT_3D ( 'NONE', #7370, #9875, #5824 ) ;
#4866 = LINE ( 'NONE', #8101, #7363 ) ;
#4867 = ORIENTED_EDGE ( 'NONE', *, *, #7734, .F. ) ;
#4868 = ORIENTED_EDGE ( 'NONE', *, *, #7098, .T. ) ;
#4869 = VERTEX_POINT ( 'NONE', #1194 ) ;
#4870 = AXIS2_PLACEMENT_3D ( 'NONE', #641, #4754, #10441 ) ;
#4871 = VERTEX_POINT ( 'NONE', #2780 ) ;
#4872 = CARTESIAN_POINT ( 'NONE',  ( -142.7649729728221359, 249.8094598553370531, 0.000000000000000000 ) ) ;
#4873 = DIRECTION ( 'NONE',  ( -0.000000000000000000, -1.000000000000000000, -0.000000000000000000 ) ) ;
#4874 = FACE_BOUND ( 'NONE', #7735, .T. ) ;
#4875 = ADVANCED_FACE ( 'NONE', ( #2038 ), #6067, .T. ) ;
#4876 = ADVANCED_FACE ( 'NONE', ( #4426 ), #355, .F. ) ;
#4877 = CARTESIAN_POINT ( 'NONE',  ( -16.29350689640809691, 105.5289575273812233, 54.43095569077609497 ) ) ;
#4878 = EDGE_CURVE ( 'NONE', #6462, #2154, #4382, .T. ) ;
#4879 = ORIENTED_EDGE ( 'NONE', *, *, #5146, .T. ) ;
#4880 = LINE ( 'NONE', #4042, #10109 ) ;
#4881 = ADVANCED_FACE ( 'NONE', ( #7661 ), #9760, .T. ) ;
#4882 = ORIENTED_EDGE ( 'NONE', *, *, #430, .T. ) ;
#4883 = AXIS2_PLACEMENT_3D ( 'NONE', #9831, #1758, #179 ) ;
#4884 = EDGE_LOOP ( 'NONE', ( #1547, #336, #18, #2877 ) ) ;
#4885 = DIRECTION ( 'NONE',  ( 0.000000000000000000, 0.000000000000000000, 1.000000000000000000 ) ) ;
#4886 = DIRECTION ( 'NONE',  ( 1.396588258780021135E-16, -0.000000000000000000, 1.000000000000000000 ) ) ;
#4887 = DIRECTION ( 'NONE',  ( 0.000000000000000000, -1.000000000000000000, 0.000000000000000000 ) ) ;
#4888 = ADVANCED_FACE ( 'NONE', ( #3636 ), #6011, .F. ) ;
#4889 = AXIS2_PLACEMENT_3D ( 'NONE', #337, #8434, #7535 ) ;
#4890 = CARTESIAN_POINT ( 'NONE',  ( 3.000000000000000000, 2.935248768560057897, -3.252606517456513302E-15 ) ) ;
#4891 = CYLINDRICAL_SURFACE ( 'NONE', #2317, 4.000000000000000000 ) ;
#4892 = ORIENTED_EDGE ( 'NONE', *, *, #745, .F. ) ;
#4893 = CARTESIAN_POINT ( 'NONE',  ( 3.000000000000000000, 1.467624384280025174, -2.542000000000001592 ) ) ;
#4894 = APPLICATION_PROTOCOL_DEFINITION ( 'draft international standard', 'automotive_design', 1998, #770 ) ;
#4895 = ORIENTED_EDGE ( 'NONE', *, *, #1456, .F. ) ;
#4896 = CARTESIAN_POINT ( 'NONE',  ( -24.41868145091758535, -134.3099331815685105, 49.99999999999998579 ) ) ;
#4897 = ORIENTED_EDGE ( 'NONE', *, *, #1799, .F. ) ;
#4898 = PLANE ( 'NONE',  #2823 ) ;
#4899 = DIRECTION ( 'NONE',  ( -1.000000000000000000, 0.000000000000000000, 0.000000000000000000 ) ) ;
#4900 = LINE ( 'NONE', #2418, #7893 ) ;
#4901 = CARTESIAN_POINT ( 'NONE',  ( 4.856471286862175774, 147.5696653505793279, -25.00000000000000355 ) ) ;
#4902 = DIRECTION ( 'NONE',  ( -0.000000000000000000, 1.000000000000000000, -0.000000000000000000 ) ) ;
#4903 = ADVANCED_FACE ( 'NONE', ( #6923 ), #1090, .T. ) ;
#4904 = ORIENTED_EDGE ( 'NONE', *, *, #4779, .F. ) ;
#4905 = CARTESIAN_POINT ( 'NONE',  ( -40.00000000000001421, -135.1707019118818778, -40.00000000000002132 ) ) ;
#4906 = CARTESIAN_POINT ( 'NONE',  ( 85.07264007511442117, 55.10093597859600578, 25.00000000000000000 ) ) ;
#4907 = DIRECTION ( 'NONE',  ( -1.396588258780021135E-16, 0.000000000000000000, 1.000000000000000000 ) ) ;
#4908 = CARTESIAN_POINT ( 'NONE',  ( 0.000000000000000000, -117.1457019118819005, 47.99999999999997868 ) ) ;
#4909 = CARTESIAN_POINT ( 'NONE',  ( -97.04168628513710360, 208.6400276031560281, 0.000000000000000000 ) ) ;
#4910 = CARTESIAN_POINT ( 'NONE',  ( -7.293506896408098683, 120.5696653505793705, 28.00000000000000355 ) ) ;
#4911 = FACE_OUTER_BOUND ( 'NONE', #7740, .T. ) ;
#4912 = VERTEX_POINT ( 'NONE', #9359 ) ;
#4913 = ORIENTED_EDGE ( 'NONE', *, *, #2682, .F. ) ;
#4914 = TOROIDAL_SURFACE ( 'NONE', #3923, 4.000000000000000000, 2.000000000000000000 ) ;
#4915 = ORIENTED_EDGE ( 'NONE', *, *, #5104, .F. ) ;
#4916 = EDGE_CURVE ( 'NONE', #2551, #3355, #6709, .T. ) ;
#4917 = EDGE_LOOP ( 'NONE', ( #6767, #1018 ) ) ;
#4918 = CARTESIAN_POINT ( 'NONE',  ( -56.36957570605427037, 137.0132282531173473, 0.000000000000000000 ) ) ;
#4919 = SURFACE_STYLE_USAGE ( .BOTH. , #5032 ) ;
#4920 = AXIS2_PLACEMENT_3D ( 'NONE', #7339, #4159, #5636 ) ;
#4921 = DIRECTION ( 'NONE',  ( 0.000000000000000000, -1.000000000000000000, 1.329743448921561232E-15 ) ) ;
#4922 = CARTESIAN_POINT ( 'NONE',  ( -2.293506896408097795, 120.5696653505793705, -20.00000000000000711 ) ) ;
#4923 = ORIENTED_EDGE ( 'NONE', *, *, #5784, .F. ) ;
#4924 = DIRECTION ( 'NONE',  ( 0.000000000000000000, 0.000000000000000000, 1.000000000000000000 ) ) ;
#4925 = ORIENTED_EDGE ( 'NONE', *, *, #2549, .F. ) ;
#4926 = PLANE ( 'NONE',  #9120 ) ;
#4927 = AXIS2_PLACEMENT_3D ( 'NONE', #531, #5453, #587 ) ;
#4928 = AXIS2_PLACEMENT_3D ( 'NONE', #4725, #1445, #7913 ) ;
#4929 = EDGE_CURVE ( 'NONE', #7226, #8168, #9145, .T. ) ;
#4930 = EDGE_CURVE ( 'NONE', #8839, #3419, #6359, .T. ) ;
#4931 = ORIENTED_EDGE ( 'NONE', *, *, #7675, .F. ) ;
#4932 = UNCERTAINTY_MEASURE_WITH_UNIT (LENGTH_MEASURE( 1.000000000000000082E-05 ), #1252, 'distance_accuracy_value', 'NONE');
#4933 = CARTESIAN_POINT ( 'NONE',  ( -20.29350689640809691, 140.5696653505793563, 20.00000000000002132 ) ) ;
#4934 = LINE ( 'NONE', #6535, #1719 ) ;
#4935 = DIRECTION ( 'NONE',  ( 0.000000000000000000, -1.222897680782651471E-16, 1.000000000000000000 ) ) ;
#4936 = DIRECTION ( 'NONE',  ( -0.6585271261848796298, 0.7525569905852207420, 0.000000000000000000 ) ) ;
#4937 = VECTOR ( 'NONE', #9321, 1000.000000000000000 ) ;
#4938 = VECTOR ( 'NONE', #4329, 1000.000000000000000 ) ;
#4939 = DIRECTION ( 'NONE',  ( 1.000000000000000000, 0.000000000000000000, -1.734723475976805615E-16 ) ) ;
#4940 = EDGE_LOOP ( 'NONE', ( #6739, #3430, #2826 ) ) ;
#4941 = DIRECTION ( 'NONE',  ( 0.000000000000000000, 0.000000000000000000, 1.000000000000000000 ) ) ;
#4942 = EDGE_CURVE ( 'NONE', #910, #4373, #6530, .T. ) ;
#4944 = EDGE_CURVE ( 'NONE', #2553, #9915, #2300, .T. ) ;
#4943 = VERTEX_POINT ( 'NONE', #9633 ) ;
#4945 = AXIS2_PLACEMENT_3D ( 'NONE', #8058, #7173, #4823 ) ;
#4946 = ADVANCED_FACE ( 'NONE', ( #8614 ), #10211, .T. ) ;
#4947 = CARTESIAN_POINT ( 'NONE',  ( -23.79350689640809691, 120.5289575273812233, 54.43095569077609497 ) ) ;
#4948 = VECTOR ( 'NONE', #1825, 1000.000000000000000 ) ;
#4949 = ORIENTED_EDGE ( 'NONE', *, *, #9190, .F. ) ;
#4950 = CARTESIAN_POINT ( 'NONE',  ( -93.80004353141508489, 205.7212393575359783, 0.000000000000000000 ) ) ;
#4951 = DIRECTION ( 'NONE',  ( -1.000000000000000000, 0.000000000000000000, 0.000000000000000000 ) ) ;
#4952 = DIRECTION ( 'NONE',  ( 0.000000000000000000, 0.000000000000000000, 1.000000000000000000 ) ) ;
#4953 = CIRCLE ( 'NONE', #5292, 8.681329343575942659 ) ;
#4954 = CARTESIAN_POINT ( 'NONE',  ( -24.29350689640808625, 140.5696653505793563, -10.98204862120179648 ) ) ;
#4955 = DIRECTION ( 'NONE',  ( 0.000000000000000000, 1.000000000000000000, 0.000000000000000000 ) ) ;
#4956 = ORIENTED_EDGE ( 'NONE', *, *, #7719, .F. ) ;
#4957 = EDGE_CURVE ( 'NONE', #39, #4985, #3151, .T. ) ;
#4958 = DIRECTION ( 'NONE',  ( 1.277197683604454965E-16, -1.000000000000000000, 0.000000000000000000 ) ) ;
#4959 = ORIENTED_EDGE ( 'NONE', *, *, #3390, .F. ) ;
#4960 = LINE ( 'NONE', #9701, #7251 ) ;
#4961 = DIRECTION ( 'NONE',  ( -0.000000000000000000, -1.000000000000000000, -0.000000000000000000 ) ) ;
#4962 = AXIS2_PLACEMENT_3D ( 'NONE', #7620, #2785, #7510 ) ;
#4963 = ORIENTED_EDGE ( 'NONE', *, *, #7689, .F. ) ;
#4964 = DIRECTION ( 'NONE',  ( 0.000000000000000000, 0.000000000000000000, 1.000000000000000000 ) ) ;
#4965 = DIRECTION ( 'NONE',  ( 0.000000000000000000, -1.000000000000000000, 0.000000000000000000 ) ) ;
#4966 = ADVANCED_FACE ( 'NONE', ( #9581 ), #3099, .T. ) ;
#4967 = CARTESIAN_POINT ( 'NONE',  ( -155.4728935706336301, 261.2517229562222951, 0.000000000000000000 ) ) ;
#4968 = LINE ( 'NONE', #5077, #1779 ) ;
#4969 = AXIS2_PLACEMENT_3D ( 'NONE', #9383, #2523, #2417 ) ;
#4970 = EDGE_LOOP ( 'NONE', ( #2956, #7579, #3948, #3745 ) ) ;
#4971 = ORIENTED_EDGE ( 'NONE', *, *, #1959, .F. ) ;
#4972 = ORIENTED_EDGE ( 'NONE', *, *, #3776, .F. ) ;
#4973 = CARTESIAN_POINT ( 'NONE',  ( -38.19229777560033057, 37.08684478514405214, -12.50000000000000000 ) ) ;
#4974 = DIRECTION ( 'NONE',  ( -1.000000000000000000, -0.000000000000000000, -0.000000000000000000 ) ) ;
#4975 = CIRCLE ( 'NONE', #3455, 26.17065043502059396 ) ;
#4976 = CARTESIAN_POINT ( 'NONE',  ( 23.76520584195949226, -145.1457019118819005, -50.00000000000002132 ) ) ;
#4977 = EDGE_CURVE ( 'NONE', #822, #510, #6382, .T. ) ;
#4978 = DIRECTION ( 'NONE',  ( 0.000000000000000000, 0.000000000000000000, -1.000000000000000000 ) ) ;
#4979 = ORIENTED_EDGE ( 'NONE', *, *, #9094, .T. ) ;
#4980 = ORIENTED_EDGE ( 'NONE', *, *, #17, .T. ) ;
#4981 = LINE ( 'NONE', #6525, #295 ) ;
#4982 = ORIENTED_EDGE ( 'NONE', *, *, #8347, .T. ) ;
#4983 = SURFACE_STYLE_FILL_AREA ( #1815 ) ;
#4984 = AXIS2_PLACEMENT_3D ( 'NONE', #5025, #9976, #4235 ) ;
#4985 = VERTEX_POINT ( 'NONE', #10368 ) ;
#4986 = ORIENTED_EDGE ( 'NONE', *, *, #2751, .F. ) ;
#4987 = FACE_OUTER_BOUND ( 'NONE', #9415, .T. ) ;
#4988 = LINE ( 'NONE', #3302, #4086 ) ;
#4989 = LINE ( 'NONE', #9944, #5849 ) ;
#4990 = DIRECTION ( 'NONE',  ( -1.000000000000000000, 7.848480207562752404E-17, 0.000000000000000000 ) ) ;
#4991 = FACE_BOUND ( 'NONE', #5354, .T. ) ;
#4992 = ADVANCED_FACE ( 'NONE', ( #5376 ), #4735, .T. ) ;
#4993 = FACE_OUTER_BOUND ( 'NONE', #3314, .T. ) ;
#4994 = CONICAL_SURFACE ( 'NONE', #1789, 4.999999999999993783, 1.029744258676652979 ) ;
#4995 = ORIENTED_EDGE ( 'NONE', *, *, #2722, .F. ) ;
#4996 = CARTESIAN_POINT ( 'NONE',  ( -23.17384457509314899, 130.5696653505793847, 10.90000000000000036 ) ) ;
#4997 = ITEM_DEFINED_TRANSFORMATION ( 'NONE', 'NONE', #7685,  #4601 ) ;
#4998 = EDGE_LOOP ( 'NONE', ( #8517, #5606, #8562, #4110 ) ) ;
#4999 = VECTOR ( 'NONE', #236, 1000.000000000000000 ) ;
#5000 = CARTESIAN_POINT ( 'NONE',  ( -23.64292728780887032, -133.6309146189979060, 49.99999999999997868 ) ) ;
#5001 = VERTEX_POINT ( 'NONE', #5481 ) ;
#5002 = AXIS2_PLACEMENT_3D ( 'NONE', #4156, #9789, #1768 ) ;
#5003 = CARTESIAN_POINT ( 'NONE',  ( -30.29350689640809335, 0.000000000000000000, 0.000000000000000000 ) ) ;
#5004 = CARTESIAN_POINT ( 'NONE',  ( -20.29350689640809691, 140.5696653505793563, -7.749999999999996447 ) ) ;
#5005 = ADVANCED_FACE ( 'NONE', ( #509 ), #4994, .F. ) ;
#5006 = EDGE_CURVE ( 'NONE', #1083, #8633, #8218, .T. ) ;
#5007 = LINE ( 'NONE', #1622, #948 ) ;
#5008 = EDGE_CURVE ( 'NONE', #8658, #6094, #5536, .T. ) ;
#5009 = DIRECTION ( 'NONE',  ( -1.000000000000000000, -0.000000000000000000, -0.000000000000000000 ) ) ;
#5010 = DIRECTION ( 'NONE',  ( 0.000000000000000000, 0.000000000000000000, 1.000000000000000000 ) ) ;
#5011 = VECTOR ( 'NONE', #5196, 1000.000000000000000 ) ;
#5012 = EDGE_CURVE ( 'NONE', #8070, #6030, #8303, .T. ) ;
#5013 = ORIENTED_EDGE ( 'NONE', *, *, #7178, .F. ) ;
#5014 = ORIENTED_EDGE ( 'NONE', *, *, #10042, .F. ) ;
#5015 = CARTESIAN_POINT ( 'NONE',  ( -16.26850689640809833, 140.5696653505793563, 7.750000000000000888 ) ) ;
#5016 = AXIS2_PLACEMENT_3D ( 'NONE', #1203, #364, #3589 ) ;
#5017 = VERTEX_POINT ( 'NONE', #561 ) ;
#5018 = CARTESIAN_POINT ( 'NONE',  ( -23.79350689640809691, 120.5289575273812233, -7.750000000000000000 ) ) ;
#5019 = CARTESIAN_POINT ( 'NONE',  ( 4.856471286862175774, 152.5696653505793279, 30.00000000000000355 ) ) ;
#5020 = CIRCLE ( 'NONE', #630, 3.999999999999999112 ) ;
#5021 = AXIS2_PLACEMENT_3D ( 'NONE', #4015, #6549, #9798 ) ;
#5022 = DIRECTION ( 'NONE',  ( 1.000000000000000000, 0.000000000000000000, -0.000000000000000000 ) ) ;
#5023 = DIRECTION ( 'NONE',  ( -0.000000000000000000, 1.000000000000000000, -0.000000000000000000 ) ) ;
#5024 = ADVANCED_FACE ( 'NONE', ( #1356 ), #4581, .F. ) ;
#5025 = CARTESIAN_POINT ( 'NONE',  ( -27.15769640663941331, -133.1457019118818721, 27.15769640663938489 ) ) ;
#5026 = VECTOR ( 'NONE', #10206, 1000.000000000000000 ) ;
#5027 = EDGE_LOOP ( 'NONE', ( #6272, #5643, #6069, #2990 ) ) ;
#5028 = B_SPLINE_CURVE_WITH_KNOTS ( 'NONE', 3,
 ( #4734, #6381, #9466, #8772, #1298, #1515, #611, #560, #7973, #714 ),
 .UNSPECIFIED., .F., .F.,
 ( 4, 2, 2, 2, 4 ),
 ( -8.944271910636758738E-06, 0.001019331502940711920, 0.002047607277792060521, 0.003075883052643409339, 0.004104158827494757723 ),
 .UNSPECIFIED. ) ;
#5029 = EDGE_LOOP ( 'NONE', ( #8827, #6816 ) ) ;
#5030 = VERTEX_POINT ( 'NONE', #3795 ) ;
#5031 = CARTESIAN_POINT ( 'NONE',  ( -8.793506896408100459, 76.32362273389503571, -7.750000000000014211 ) ) ;
#5032 = SURFACE_SIDE_STYLE ('',( #8962 ) ) ;
#5033 = AXIS2_PLACEMENT_3D ( 'NONE', #4619, #7855, #6519 ) ;
#5034 = LINE ( 'NONE', #4141, #7494 ) ;
#5035 = DIRECTION ( 'NONE',  ( 1.000000000000000000, 0.000000000000000000, -0.000000000000000000 ) ) ;
#5036 = EDGE_LOOP ( 'NONE', ( #6393, #7969, #5560, #10029 ) ) ;
#5037 = DIRECTION ( 'NONE',  ( 0.000000000000000000, -1.000000000000000000, 0.000000000000000000 ) ) ;
#5038 = ORIENTED_EDGE ( 'NONE', *, *, #4108, .F. ) ;
#5039 = SURFACE_STYLE_USAGE ( .BOTH. , #5199 ) ;
#5040 = AXIS2_PLACEMENT_3D ( 'NONE', #329, #9168, #6729 ) ;
#5041 = EDGE_CURVE ( 'NONE', #4464, #264, #1618, .T. ) ;
#5042 = EDGE_LOOP ( 'NONE', ( #6570, #4844, #10127, #2290 ) ) ;
#5043 = CIRCLE ( 'NONE', #485, 2.000000000000001776 ) ;
#5044 = PRODUCT_DEFINITION_CONTEXT ( 'detailed design', #2265, 'design' ) ;
#5045 = LINE ( 'NONE', #860, #8595 ) ;
#5046 = DIRECTION ( 'NONE',  ( 1.000000000000000000, -0.000000000000000000, -0.000000000000000000 ) ) ;
#5047 = DIRECTION ( 'NONE',  ( -0.000000000000000000, -1.000000000000000000, -0.000000000000000000 ) ) ;
#5048 = VECTOR ( 'NONE', #8042, 1000.000000000000000 ) ;
#5049 = CARTESIAN_POINT ( 'NONE',  ( -30.29350689640809335, 2.445795361565304815E-15, 20.00000000000002132 ) ) ;
#5050 = DIRECTION ( 'NONE',  ( 0.000000000000000000, 0.000000000000000000, -1.000000000000000000 ) ) ;
#5051 = ORIENTED_EDGE ( 'NONE', *, *, #678, .F. ) ;
#5052 = AXIS2_PLACEMENT_3D ( 'NONE', #1138, #3575, #6111 ) ;
#5053 = CYLINDRICAL_SURFACE ( 'NONE', #6138, 3.297986701801175258 ) ;
#5054 = ORIENTED_EDGE ( 'NONE', *, *, #428, .F. ) ;
#5055 = ADVANCED_BREP_SHAPE_REPRESENTATION ( '', ( #3077, #4601 ), #9214 ) ;
#5056 = LINE ( 'NONE', #87, #3711 ) ;
#5057 = ADVANCED_FACE ( 'NONE', ( #7929 ), #2996, .T. ) ;
#5058 = VERTEX_POINT ( 'NONE', #5428 ) ;
#5059 = AXIS2_PLACEMENT_3D ( 'NONE', #6565, #7415, #8207 ) ;
#5060 = CARTESIAN_POINT ( 'NONE',  ( 99.80027788547049283, -145.1457019118819005, 25.00000000000000000 ) ) ;
#5061 = CARTESIAN_POINT ( 'NONE',  ( -21.44003972449636208, -143.0117419471019673, -6.332076144530982553 ) ) ;
#5062 = DIRECTION ( 'NONE',  ( 1.000000000000000000, 7.848480207562752404E-17, -0.000000000000000000 ) ) ;
#5063 = FACE_OUTER_BOUND ( 'NONE', #2952, .T. ) ;
#5064 = CARTESIAN_POINT ( 'NONE',  ( -43.93820948810023452, 0.000000000000000000, 0.000000000000000000 ) ) ;
#5065 = MECHANICAL_DESIGN_GEOMETRIC_PRESENTATION_REPRESENTATION (  '', ( #6941 ), #1523 ) ;
#5066 = VERTEX_POINT ( 'NONE', #8664 ) ;
#5067 = LINE ( 'NONE', #9050, #7736 ) ;
#5068 = SHAPE_REPRESENTATION ( 'socket head cap screw_iso_ISO 4762 M6 x 20 - 20N', ( #4601 ), #3113 ) ;
#5069 = EDGE_CURVE ( 'NONE', #1149, #6373, #3905, .T. ) ;
#5070 = EDGE_CURVE ( 'NONE', #2663, #84, #5340, .T. ) ;
#5071 = ORIENTED_EDGE ( 'NONE', *, *, #4977, .F. ) ;
#5072 = CARTESIAN_POINT ( 'NONE',  ( 1.940506014114293224E-14, -117.1457019118819005, -23.15769640663941331 ) ) ;
#5073 = DIRECTION ( 'NONE',  ( 0.000000000000000000, 1.000000000000000000, 0.000000000000000000 ) ) ;
#5074 = DIRECTION ( 'NONE',  ( 0.000000000000000000, 0.000000000000000000, -1.000000000000000000 ) ) ;
#5075 = DIRECTION ( 'NONE',  ( 0.000000000000000000, 0.000000000000000000, 1.000000000000000000 ) ) ;
#5076 = DIRECTION ( 'NONE',  ( 0.000000000000000000, 0.000000000000000000, 1.000000000000000000 ) ) ;
#5077 = CARTESIAN_POINT ( 'NONE',  ( 25.15769640663937778, -115.1457019118818863, -23.15769640663940976 ) ) ;
#5078 = ORIENTED_EDGE ( 'NONE', *, *, #7379, .T. ) ;
#5079 = EDGE_LOOP ( 'NONE', ( #6218, #2387, #8316, #8023 ) ) ;
#5080 = PRODUCT_RELATED_PRODUCT_CATEGORY ( 'part', '', ( #7048 ) ) ;
#5081 = ADVANCED_FACE ( 'NONE', ( #4993 ), #6198, .F. ) ;
#5082 = EDGE_CURVE ( 'NONE', #1253, #5224, #82, .T. ) ;
#5083 = ORIENTED_EDGE ( 'NONE', *, *, #5478, .T. ) ;
#5084 = ADVANCED_FACE ( 'NONE', ( #8236, #7235 ), #5794, .T. ) ;
#5085 = ORIENTED_EDGE ( 'NONE', *, *, #8829, .T. ) ;
#5086 = CARTESIAN_POINT ( 'NONE',  ( -39.65557114539779349, 0.1824758893689546746, 3.996877754856924536 ) ) ;
#5087 = FACE_OUTER_BOUND ( 'NONE', #4970, .T. ) ;
#5088 = CARTESIAN_POINT ( 'NONE',  ( -57.23930847856151161, 167.4192747350194850, 0.000000000000000000 ) ) ;
#5089 = DIRECTION ( 'NONE',  ( -0.7431448254773957984, 0.6691306063588565722, -0.000000000000000000 ) ) ;
#5090 = AXIS2_PLACEMENT_3D ( 'NONE', #3871, #5600, #1577 ) ;
#5091 = ORIENTED_EDGE ( 'NONE', *, *, #3218, .T. ) ;
#5092 = DIRECTION ( 'NONE',  ( 0.7431448254773962425, -0.6691306063588559061, 0.000000000000000000 ) ) ;
#5093 = ORIENTED_EDGE ( 'NONE', *, *, #2684, .T. ) ;
#5094 = DIRECTION ( 'NONE',  ( 6.106226635438360972E-16, -1.000000000000000000, 0.000000000000000000 ) ) ;
#5095 = ORIENTED_EDGE ( 'NONE', *, *, #6587, .T. ) ;
#5096 = EDGE_CURVE ( 'NONE', #7140, #2630, #7215, .T. ) ;
#5097 = VECTOR ( 'NONE', #495, 1000.000000000000000 ) ;
#5098 = ORIENTED_EDGE ( 'NONE', *, *, #5667, .F. ) ;
#5099 = LINE ( 'NONE', #4305, #7399 ) ;
#5100 = LINE ( 'NONE', #5787, #1034 ) ;
#5101 = DIRECTION ( 'NONE',  ( -0.000000000000000000, -0.000000000000000000, -1.000000000000000000 ) ) ;
#5102 = DIRECTION ( 'NONE',  ( -7.848480207562752404E-17, -1.000000000000000000, 0.000000000000000000 ) ) ;
#5103 = DIRECTION ( 'NONE',  ( -1.000000000000000000, -0.000000000000000000, -0.000000000000000000 ) ) ;
#5104 = EDGE_CURVE ( 'NONE', #5655, #898, #3200, .T. ) ;
#5105 = CARTESIAN_POINT ( 'NONE',  ( -16.29350689640809691, 88.12362273389504708, 0.000000000000000000 ) ) ;
#5106 = AXIS2_PLACEMENT_3D ( 'NONE', #3736, #4778, #6965 ) ;
#5107 = APPLICATION_CONTEXT ( 'automotive_design' ) ;
#5108 = EDGE_LOOP ( 'NONE', ( #6742, #5876, #5051, #1718, #3857 ) ) ;
#5109 = VECTOR ( 'NONE', #5881, 1000.000000000000000 ) ;
#5110 = DIRECTION ( 'NONE',  ( -0.000000000000000000, 1.000000000000000000, -0.000000000000000000 ) ) ;
#5111 = VERTEX_POINT ( 'NONE', #4838 ) ;
#5112 = DIRECTION ( 'NONE',  ( 0.000000000000000000, -1.000000000000000000, 0.000000000000000000 ) ) ;
#5113 = ORIENTED_EDGE ( 'NONE', *, *, #2873, .F. ) ;
#5114 = CIRCLE ( 'NONE', #549, 7.500000000000000000 ) ;
#5115 = AXIS2_PLACEMENT_3D ( 'NONE', #10420, #7820, #4787 ) ;
#5116 = DIRECTION ( 'NONE',  ( -0.000000000000000000, -1.000000000000000000, -0.000000000000000000 ) ) ;
#5117 = DIRECTION ( 'NONE',  ( 0.000000000000000000, 0.000000000000000000, 1.000000000000000000 ) ) ;
#5118 = DIRECTION ( 'NONE',  ( -1.000000000000000000, -0.000000000000000000, -0.000000000000000000 ) ) ;
#5119 = FACE_OUTER_BOUND ( 'NONE', #3288, .T. ) ;
#5120 = ORIENTED_EDGE ( 'NONE', *, *, #8198, .F. ) ;
#5121 = CIRCLE ( 'NONE', #8338, 4.729641367753003145 ) ;
#5122 = AXIS2_PLACEMENT_3D ( 'NONE', #29, #5740, #5796 ) ;
#5123 = EDGE_LOOP ( 'NONE', ( #9060, #1585, #159, #8172 ) ) ;
#5124 = CARTESIAN_POINT ( 'NONE',  ( -21.29350689640810401, 105.5289575273812233, 7.750000000000000888 ) ) ;
#5125 = ORIENTED_EDGE ( 'NONE', *, *, #414, .F. ) ;
#5126 = CARTESIAN_POINT ( 'NONE',  ( -20.29350689640809691, 140.5696653505793563, 19.97500000000000853 ) ) ;
#5127 = PLANE ( 'NONE',  #2574 ) ;
#5128 = AXIS2_PLACEMENT_3D ( 'NONE', #1489, #1540, #10444 ) ;
#5129 = DIRECTION ( 'NONE',  ( -1.000000000000000000, -0.000000000000000000, -0.000000000000000000 ) ) ;
#5130 = FACE_OUTER_BOUND ( 'NONE', #5580, .T. ) ;
#5131 = DIRECTION ( 'NONE',  ( 0.000000000000000000, 0.000000000000000000, -1.000000000000000000 ) ) ;
#5132 = DIRECTION ( 'NONE',  ( -1.000000000000000000, 0.000000000000000000, -0.000000000000000000 ) ) ;
#5133 = EDGE_CURVE ( 'NONE', #822, #5783, #5684, .T. ) ;
#5134 = ORIENTED_EDGE ( 'NONE', *, *, #2161, .T. ) ;
#5135 = ORIENTED_EDGE ( 'NONE', *, *, #6294, .T. ) ;
#5136 = CIRCLE ( 'NONE', #6150, 2.000000000000001776 ) ;
#5137 = DIRECTION ( 'NONE',  ( 0.000000000000000000, 0.000000000000000000, 1.000000000000000000 ) ) ;
#5138 = CARTESIAN_POINT ( 'NONE',  ( -50.00000000000002132, -134.3099192498709158, 24.41866285951200766 ) ) ;
#5139 = DIRECTION ( 'NONE',  ( -1.000000000000000000, -0.000000000000000000, -0.000000000000000000 ) ) ;
#5140 = VECTOR ( 'NONE', #8990, 1000.000000000000000 ) ;
#5141 = ORIENTED_EDGE ( 'NONE', *, *, #3206, .F. ) ;
#5142 = EDGE_CURVE ( 'NONE', #910, #5311, #1966, .T. ) ;
#5143 = CARTESIAN_POINT ( 'NONE',  ( -16.29350689640809691, 55.56966535057936341, 0.000000000000000000 ) ) ;
#5144 = EDGE_CURVE ( 'NONE', #5066, #5352, #974, .T. ) ;
#5145 =( GEOMETRIC_REPRESENTATION_CONTEXT ( 3 ) GLOBAL_UNCERTAINTY_ASSIGNED_CONTEXT ( ( #8973 ) ) GLOBAL_UNIT_ASSIGNED_CONTEXT ( ( #7876, #7978, #3050 ) ) REPRESENTATION_CONTEXT ( 'NONE', 'WORKASPACE' ) );
#5146 = EDGE_CURVE ( 'NONE', #9448, #9884, #6364, .T. ) ;
#5147 = ORIENTED_EDGE ( 'NONE', *, *, #3218, .F. ) ;
#5148 = AXIS2_PLACEMENT_3D ( 'NONE', #8558, #6974, #6168 ) ;
#5149 = ORIENTED_EDGE ( 'NONE', *, *, #5381, .F. ) ;
#5150 = CARTESIAN_POINT ( 'NONE',  ( -30.29350689640809335, 2.445795361565304815E-15, 20.00000000000002132 ) ) ;
#5151 = PLANE ( 'NONE',  #3748 ) ;
#5152 = CARTESIAN_POINT ( 'NONE',  ( 23.15769640663938134, -115.1457019118818863, -27.15769640663941686 ) ) ;
#5153 = LINE ( 'NONE', #4367, #1222 ) ;
#5154 = PLANE ( 'NONE',  #2442 ) ;
#5155 = DIRECTION ( 'NONE',  ( 0.000000000000000000, 0.000000000000000000, 1.000000000000000000 ) ) ;
#5156 = AXIS2_PLACEMENT_3D ( 'NONE', #2434, #9498, #8899 ) ;
#5157 = ADVANCED_FACE ( 'NONE', ( #3252 ), #10270, .T. ) ;
#5158 = EDGE_LOOP ( 'NONE', ( #4845, #486, #4753, #3287 ) ) ;
#5159 = CARTESIAN_POINT ( 'NONE',  ( 25.44550000000000978, 0.000000000000000000, 0.000000000000000000 ) ) ;
#5160 = ORIENTED_EDGE ( 'NONE', *, *, #10204, .F. ) ;
#5161 = CARTESIAN_POINT ( 'NONE',  ( 10.51964330236497602, 150.0000000000000000, 25.00000000000000000 ) ) ;
#5162 = VERTEX_POINT ( 'NONE', #138 ) ;
#5163 = APPLICATION_CONTEXT ( 'automotive_design' ) ;
#5164 = FACE_OUTER_BOUND ( 'NONE', #2095, .T. ) ;
#5165 = FACE_OUTER_BOUND ( 'NONE', #2528, .T. ) ;
#5166 = DIRECTION ( 'NONE',  ( -0.6691306063588561281, -0.7431448254773961315, 0.000000000000000000 ) ) ;
#5167 = DIRECTION ( 'NONE',  ( -7.061912783291096091E-17, 0.08715574274765486296, 0.9961946980917459893 ) ) ;
#5168 = ORIENTED_EDGE ( 'NONE', *, *, #1949, .F. ) ;
#5169 = FACE_OUTER_BOUND ( 'NONE', #4197, .T. ) ;
#5170 =( NAMED_UNIT ( * ) SI_UNIT ( $, .STERADIAN. ) SOLID_ANGLE_UNIT ( ) );
#5171 = ORIENTED_EDGE ( 'NONE', *, *, #6432, .F. ) ;
#5172 = LINE ( 'NONE', #9208, #3505 ) ;
#5173 = EDGE_CURVE ( 'NONE', #8863, #10023, #1668, .T. ) ;
#5174 = ORIENTED_EDGE ( 'NONE', *, *, #3992, .F. ) ;
#5175 = DIRECTION ( 'NONE',  ( -0.000000000000000000, -0.000000000000000000, -1.000000000000000000 ) ) ;
#5176 = DIRECTION ( 'NONE',  ( 1.000000000000000000, 0.000000000000000000, -0.000000000000000000 ) ) ;
#5177 = EDGE_LOOP ( 'NONE', ( #3106, #6299, #6172, #3913 ) ) ;
#5178 = VECTOR ( 'NONE', #320, 1000.000000000000000 ) ;
#5179 = LINE ( 'NONE', #2901, #3198 ) ;
#5180 = DIRECTION ( 'NONE',  ( 0.000000000000000000, 0.000000000000000000, 1.000000000000000000 ) ) ;
#5181 = DIRECTION ( 'NONE',  ( -0.000000000000000000, 0.000000000000000000, -1.000000000000000000 ) ) ;
#5182 = AXIS2_PLACEMENT_3D ( 'NONE', #3838, #2081, #659 ) ;
#5183 = CARTESIAN_POINT ( 'NONE',  ( -16.29350689640809691, -115.1457019118818863, 27.01918567566963247 ) ) ;
#5184 = VERTEX_POINT ( 'NONE', #3412 ) ;
#5185 = ORIENTED_EDGE ( 'NONE', *, *, #239, .T. ) ;
#5186 = AXIS2_PLACEMENT_3D ( 'NONE', #600, #4677, #3834 ) ;
#5187 = VECTOR ( 'NONE', #5037, 1000.000000000000000 ) ;
#5188 = AXIS2_PLACEMENT_3D ( 'NONE', #3476, #1244, #9198 ) ;
#5189 = VERTEX_POINT ( 'NONE', #8872 ) ;
#5190 = ADVANCED_FACE ( 'NONE', ( #9680 ), #4891, .T. ) ;
#5191 = LINE ( 'NONE', #8426, #2841 ) ;
#5192 = DIRECTION ( 'NONE',  ( -1.387778780781445676E-16, 0.000000000000000000, 1.000000000000000000 ) ) ;
#5193 = DIRECTION ( 'NONE',  ( 0.000000000000000000, -1.000000000000000000, 0.000000000000000000 ) ) ;
#5194 = VECTOR ( 'NONE', #8565, 1000.000000000000000 ) ;
#5195 = ORIENTED_EDGE ( 'NONE', *, *, #9887, .F. ) ;
#5196 = DIRECTION ( 'NONE',  ( 1.000000000000000000, 0.000000000000000000, 0.000000000000000000 ) ) ;
#5197 = VERTEX_POINT ( 'NONE', #6647 ) ;
#5198 = CIRCLE ( 'NONE', #3688, 8.681329343575942659 ) ;
#5199 = SURFACE_SIDE_STYLE ('',( #1176 ) ) ;
#5200 = TOROIDAL_SURFACE ( 'NONE', #5701, 3.250000000000000444, 0.2500000000000000000 ) ;
#5201 = ORIENTED_EDGE ( 'NONE', *, *, #6481, .T. ) ;
#5202 = EDGE_CURVE ( 'NONE', #36, #7357, #2623, .T. ) ;
#5203 = CARTESIAN_POINT ( 'NONE',  ( -8.000000000000000000, 0.000000000000000000, 0.000000000000000000 ) ) ;
#5204 = DIRECTION ( 'NONE',  ( -0.07334937666141724821, 0.9973063064792989652, 0.000000000000000000 ) ) ;
#5205 = ADVANCED_FACE ( 'NONE', ( #6694 ), #1872, .F. ) ;
#5206 = EDGE_CURVE ( 'NONE', #382, #7686, #7521, .T. ) ;
#5207 = VECTOR ( 'NONE', #7374, 1000.000000000000000 ) ;
#5208 = CARTESIAN_POINT ( 'NONE',  ( 6.756858349438876310, 146.7073643690755773, -25.00000000000000355 ) ) ;
#5209 = FACE_OUTER_BOUND ( 'NONE', #9931, .T. ) ;
#5210 = CARTESIAN_POINT ( 'NONE',  ( -168.7559887226705655, 267.8293446334838563, 0.000000000000000000 ) ) ;
#5211 = AXIS2_PLACEMENT_3D ( 'NONE', #7067, #7270, #9453 ) ;
#5212 = ORIENTED_EDGE ( 'NONE', *, *, #7195, .T. ) ;
#5213 = CARTESIAN_POINT ( 'NONE',  ( -48.00000000000002132, -117.1457019118819005, 23.15769640663938134 ) ) ;
#5214 = ORIENTED_EDGE ( 'NONE', *, *, #6119, .T. ) ;
#5215 = DIRECTION ( 'NONE',  ( 0.000000000000000000, 0.000000000000000000, -1.000000000000000000 ) ) ;
#5216 = PRODUCT_RELATED_PRODUCT_CATEGORY ( 'part', '', ( #8052 ) ) ;
#5217 = CARTESIAN_POINT ( 'NONE',  ( -2.293506896408097795, 80.56966535057935630, 16.00000000000000711 ) ) ;
#5218 = EDGE_CURVE ( 'NONE', #2498, #8078, #4508, .T. ) ;
#5219 = CIRCLE ( 'NONE', #7090, 2.000000000000001776 ) ;
#5220 = ADVANCED_FACE ( 'NONE', ( #8494 ), #6911, .T. ) ;
#5221 = CARTESIAN_POINT ( 'NONE',  ( 17.97972049165455388, 17.84145331825995484, -30.00000000000000355 ) ) ;
#5222 = CARTESIAN_POINT ( 'NONE',  ( 37.25871876463539678, -134.3867942047928921, 25.58368939469043468 ) ) ;
#5223 = CARTESIAN_POINT ( 'NONE',  ( -54.56278605312608931, 170.3918540369290895, 0.000000000000000000 ) ) ;
#5224 = VERTEX_POINT ( 'NONE', #9297 ) ;
#5225 = DIRECTION ( 'NONE',  ( -1.000000000000000000, 0.000000000000000000, 0.000000000000000000 ) ) ;
#5226 = VERTEX_POINT ( 'NONE', #5944 ) ;
#5227 = ORIENTED_EDGE ( 'NONE', *, *, #6434, .T. ) ;
#5228 = DIRECTION ( 'NONE',  ( 0.000000000000000000, -1.000000000000000000, -1.222897680782651224E-16 ) ) ;
#5229 = AXIS2_PLACEMENT_3D ( 'NONE', #4420, #2775, #10205 ) ;
#5230 = VERTEX_POINT ( 'NONE', #10094 ) ;
#5231 = CARTESIAN_POINT ( 'NONE',  ( 59.99999999999997868, 52.77167129626698028, 40.00000000000000000 ) ) ;
#5232 = CARTESIAN_POINT ( 'NONE',  ( 23.15769640663936713, -117.1457019118819005, 49.99999999999997868 ) ) ;
#5233 = DIRECTION ( 'NONE',  ( 0.000000000000000000, 0.000000000000000000, 1.000000000000000000 ) ) ;
#5234 = DIRECTION ( 'NONE',  ( 0.000000000000000000, 0.000000000000000000, 1.000000000000000000 ) ) ;
#5235 = DIRECTION ( 'NONE',  ( -0.000000000000000000, 0.000000000000000000, 1.000000000000000000 ) ) ;
#5236 = CIRCLE ( 'NONE', #5403, 4.700000000000000178 ) ;
#5237 = ADVANCED_FACE ( 'NONE', ( #448 ), #7648, .T. ) ;
#5238 = ADVANCED_FACE ( 'NONE', ( #5999 ), #1077, .F. ) ;
#5239 = ORIENTED_EDGE ( 'NONE', *, *, #7737, .T. ) ;
#5240 = ORIENTED_EDGE ( 'NONE', *, *, #5611, .T. ) ;
#5241 = DIRECTION ( 'NONE',  ( 0.000000000000000000, 0.000000000000000000, 1.000000000000000000 ) ) ;
#5242 = ORIENTED_EDGE ( 'NONE', *, *, #9228, .F. ) ;
#5243 = DIRECTION ( 'NONE',  ( -0.08084652178105138087, 0.4212348471733671218, 0.9033410449230877548 ) ) ;
#5244 = DIRECTION ( 'NONE',  ( -1.000000000000000000, -0.000000000000000000, -0.000000000000000000 ) ) ;
#5245 = DIRECTION ( 'NONE',  ( 0.000000000000000000, 0.000000000000000000, 1.000000000000000000 ) ) ;
#5246 = FACE_OUTER_BOUND ( 'NONE', #4133, .T. ) ;
#5247 = ORIENTED_EDGE ( 'NONE', *, *, #3658, .T. ) ;
#5248 = EDGE_LOOP ( 'NONE', ( #7275, #1004, #7975, #7562, #3482 ) ) ;
#5249 = CARTESIAN_POINT ( 'NONE',  ( 25.15769640663935292, -133.1457019118818721, 2.459446039362539254E-14 ) ) ;
#5250 = VERTEX_POINT ( 'NONE', #10148 ) ;
#5251 = CARTESIAN_POINT ( 'NONE',  ( -7.293506896408105789, 112.5696653505793705, 20.00000000000000711 ) ) ;
#5252 = FACE_OUTER_BOUND ( 'NONE', #8081, .T. ) ;
#5253 = DIRECTION ( 'NONE',  ( -8.194486552889013533E-17, -9.100899318238110877E-17, 1.000000000000000000 ) ) ;
#5254 = DIRECTION ( 'NONE',  ( 0.000000000000000000, 0.000000000000000000, 1.000000000000000000 ) ) ;
#5255 = DIRECTION ( 'NONE',  ( -0.7431448254773957984, 0.6691306063588565722, -0.000000000000000000 ) ) ;
#5256 = ORIENTED_EDGE ( 'NONE', *, *, #7437, .F. ) ;
#5257 = DIRECTION ( 'NONE',  ( -0.000000000000000000, -0.000000000000000000, -1.000000000000000000 ) ) ;
#5258 = EDGE_CURVE ( 'NONE', #2699, #5289, #6798, .T. ) ;
#5259 = AXIS2_PLACEMENT_3D ( 'NONE', #988, #9854, #1783 ) ;
#5260 = DIRECTION ( 'NONE',  ( 0.000000000000000000, -1.000000000000000000, -1.222897680782651224E-16 ) ) ;
#5261 = CARTESIAN_POINT ( 'NONE',  ( -38.96131932220313132, 3.592756407884963199, -1.758437202063674487 ) ) ;
#5262 = TOROIDAL_SURFACE ( 'NONE', #4260, 12.02085523418795177, 4.295524112943378547 ) ;
#5263 = FACE_OUTER_BOUND ( 'NONE', #2476, .T. ) ;
#5264 = AXIS2_PLACEMENT_3D ( 'NONE', #2025, #6958, #10195 ) ;
#5265 = CARTESIAN_POINT ( 'NONE',  ( 37.24329735151886211, -134.1666765793263778, 25.43275615213076790 ) ) ;
#5266 = CARTESIAN_POINT ( 'NONE',  ( -23.76520584195948516, -145.1457019118819005, -97.78965767959371647 ) ) ;
#5267 = FACE_OUTER_BOUND ( 'NONE', #517, .T. ) ;
#5268 = VERTEX_POINT ( 'NONE', #2670 ) ;
#5269 = DIRECTION ( 'NONE',  ( 1.000000000000000000, 0.000000000000000000, 0.000000000000000000 ) ) ;
#5270 = EDGE_CURVE ( 'NONE', #7848, #6574, #2876, .T. ) ;
#5271 = EDGE_CURVE ( 'NONE', #2209, #6087, #4681, .T. ) ;
#5272 = EDGE_CURVE ( 'NONE', #2212, #493, #5346, .T. ) ;
#5273 = ORIENTED_EDGE ( 'NONE', *, *, #2171, .T. ) ;
#5274 = ORIENTED_EDGE ( 'NONE', *, *, #3924, .T. ) ;
#5275 = VECTOR ( 'NONE', #4100, 1000.000000000000000 ) ;
#5276 = CARTESIAN_POINT ( 'NONE',  ( -30.29350689640809335, 80.56966535057935630, 20.00000000000000711 ) ) ;
#5277 = AXIS2_PLACEMENT_3D ( 'NONE', #9927, #9876, #9119 ) ;
#5278 = EDGE_LOOP ( 'NONE', ( #2239, #4187, #5901, #3238, #9331 ) ) ;
#5279 = ORIENTED_EDGE ( 'NONE', *, *, #9553, .T. ) ;
#5280 = DIRECTION ( 'NONE',  ( -1.000000000000000000, 0.000000000000000000, -8.379529552680124346E-16 ) ) ;
#5281 = LINE ( 'NONE', #1045, #4937 ) ;
#5282 = SURFACE_SIDE_STYLE ('',( #7728 ) ) ;
#5283 = CYLINDRICAL_SURFACE ( 'NONE', #2269, 5.000000000000004441 ) ;
#5284 = DIRECTION ( 'NONE',  ( 1.000000000000000000, 0.000000000000000000, 0.000000000000000000 ) ) ;
#5285 = VECTOR ( 'NONE', #4413, 1000.000000000000000 ) ;
#5286 = DIRECTION ( 'NONE',  ( -0.000000000000000000, 1.000000000000000000, -0.000000000000000000 ) ) ;
#5287 = CIRCLE ( 'NONE', #1229, 5.000000000000000000 ) ;
#5288 = EDGE_CURVE ( 'NONE', #1218, #389, #285, .T. ) ;
#5289 = VERTEX_POINT ( 'NONE', #1978 ) ;
#5290 = ORIENTED_EDGE ( 'NONE', *, *, #2625, .T. ) ;
#5291 = CARTESIAN_POINT ( 'NONE',  ( -16.29350689640810756, 140.5696653505793563, 10.98204862120179826 ) ) ;
#5292 = AXIS2_PLACEMENT_3D ( 'NONE', #6949, #4558, #6038 ) ;
#5293 = ORIENTED_EDGE ( 'NONE', *, *, #9517, .F. ) ;
#5294 = DIRECTION ( 'NONE',  ( 1.000000000000000000, 0.000000000000000000, 1.734723475976805517E-15 ) ) ;
#5295 = CIRCLE ( 'NONE', #4358, 4.295524112943372330 ) ;
#5296 = CARTESIAN_POINT ( 'NONE',  ( 37.22511195853868315, -116.6161171811496189, -25.10513196898124377 ) ) ;
#5297 = CARTESIAN_POINT ( 'NONE',  ( -39.66851723004002395, -4.408728476930471151E-16, 3.600000000000004530 ) ) ;
#5298 = ORIENTED_EDGE ( 'NONE', *, *, #2943, .T. ) ;
#5299 = CIRCLE ( 'NONE', #8351, 4.000000000000003553 ) ;
#5300 = EDGE_LOOP ( 'NONE', ( #6020, #6, #7229, #2864 ) ) ;
#5301 = ORIENTED_EDGE ( 'NONE', *, *, #1453, .F. ) ;
#5302 = VERTEX_POINT ( 'NONE', #5210 ) ;
#5303 = DIRECTION ( 'NONE',  ( 0.000000000000000000, 1.000000000000000000, -1.460512169908342690E-16 ) ) ;
#5304 = EDGE_CURVE ( 'NONE', #8341, #8447, #5, .T. ) ;
#5305 = CARTESIAN_POINT ( 'NONE',  ( -23.15769640663940976, -117.1457019118819005, 47.99999999999997868 ) ) ;
#5306 = VECTOR ( 'NONE', #3376, 1000.000000000000114 ) ;
#5307 = CARTESIAN_POINT ( 'NONE',  ( -113.6864418536728465, 239.8026890743979322, 1.472130188556198457E-15 ) ) ;
#5308 = DIRECTION ( 'NONE',  ( 0.000000000000000000, 0.000000000000000000, -1.000000000000000000 ) ) ;
#5309 = AXIS2_PLACEMENT_3D ( 'NONE', #10112, #3641, #10055 ) ;
#5310 = PLANE ( 'NONE',  #5522 ) ;
#5311 = VERTEX_POINT ( 'NONE', #1238 ) ;
#5312 = DIRECTION ( 'NONE',  ( 0.000000000000000000, 0.000000000000000000, 1.000000000000000000 ) ) ;
#5313 = TOROIDAL_SURFACE ( 'NONE', #5650, 3.377784142883041074, 6.382478589986769535 ) ;
#5314 = AXIS2_PLACEMENT_3D ( 'NONE', #4445, #6991, #6027 ) ;
#5315 = CARTESIAN_POINT ( 'NONE',  ( -30.29350689640809335, 120.5696653505793705, -20.00000000000000711 ) ) ;
#5316 = ORIENTED_EDGE ( 'NONE', *, *, #9817, .F. ) ;
#5317 = EDGE_CURVE ( 'NONE', #7162, #8567, #6705, .T. ) ;
#5318 = CIRCLE ( 'NONE', #756, 9.050254677131441383 ) ;
#5319 = CARTESIAN_POINT ( 'NONE',  ( 17.97972049165455388, 37.08684478514406635, 25.00000000000000000 ) ) ;
#5320 = DIRECTION ( 'NONE',  ( 0.000000000000000000, 0.000000000000000000, 1.000000000000000000 ) ) ;
#5321 = LINE ( 'NONE', #8559, #10426 ) ;
#5322 = EDGE_LOOP ( 'NONE', ( #1334, #1891, #7324, #4831 ) ) ;
#5323 = CIRCLE ( 'NONE', #6516, 4.000000000000000000 ) ;
#5324 = DIRECTION ( 'NONE',  ( -0.000000000000000000, -1.000000000000000000, -0.000000000000000000 ) ) ;
#5325 = ORIENTED_EDGE ( 'NONE', *, *, #5641, .F. ) ;
#5326 = ORIENTED_EDGE ( 'NONE', *, *, #5728, .F. ) ;
#5327 = DIRECTION ( 'NONE',  ( -1.396588258780021135E-16, 0.000000000000000000, -1.000000000000000000 ) ) ;
#5328 = ORIENTED_EDGE ( 'NONE', *, *, #2091, .T. ) ;
#5329 = AXIS2_PLACEMENT_3D ( 'NONE', #8885, #7456, #4952 ) ;
#5330 = EDGE_LOOP ( 'NONE', ( #6438, #5195, #886, #9735 ) ) ;
#5331 = CARTESIAN_POINT ( 'NONE',  ( -7.293506896408097795, 145.5696653505793563, -20.00000000000000711 ) ) ;
#5332 = EDGE_CURVE ( 'NONE', #86, #939, #8053, .T. ) ;
#5333 = CARTESIAN_POINT ( 'NONE',  ( -100.3101032970751305, 278.5371544123273111, 0.000000000000000000 ) ) ;
#5334 = EDGE_CURVE ( 'NONE', #3261, #4722, #10197, .T. ) ;
#5335 = EDGE_CURVE ( 'NONE', #9948, #2404, #620, .T. ) ;
#5336 = DIRECTION ( 'NONE',  ( -0.000000000000000000, 1.000000000000000000, -0.000000000000000000 ) ) ;
#5337 = CYLINDRICAL_SURFACE ( 'NONE', #7179, 4.000000000000000000 ) ;
#5338 = DIRECTION ( 'NONE',  ( 0.000000000000000000, 0.000000000000000000, 1.000000000000000000 ) ) ;
#5339 = DIRECTION ( 'NONE',  ( 0.000000000000000000, -0.000000000000000000, 1.000000000000000000 ) ) ;
#5340 = CIRCLE ( 'NONE', #769, 4.024999999999997691 ) ;
#5341 = ORIENTED_EDGE ( 'NONE', *, *, #5727, .F. ) ;
#5342 = DIRECTION ( 'NONE',  ( 0.000000000000000000, 0.000000000000000000, 1.000000000000000000 ) ) ;
#5343 = CIRCLE ( 'NONE', #1458, 4.000000000000003553 ) ;
#5344 = ORIENTED_EDGE ( 'NONE', *, *, #8331, .F. ) ;
#5345 = CARTESIAN_POINT ( 'NONE',  ( -2.293506896408097795, 42.08684478514410188, 30.00000000000000355 ) ) ;
#5346 = CIRCLE ( 'NONE', #7554, 5.000000000000007994 ) ;
#5347 = EDGE_CURVE ( 'NONE', #7785, #8880, #9767, .T. ) ;
#5348 = CARTESIAN_POINT ( 'NONE',  ( 14.70649310359190309, 80.56966535057935630, -20.00000000000000711 ) ) ;
#5349 =( BOUNDED_CURVE ( )  B_SPLINE_CURVE ( 3, ( #5060, #8295, #1033, #4270 ),
 .UNSPECIFIED., .F., .T. ) 
 B_SPLINE_CURVE_WITH_KNOTS ( ( 4, 4 ),
 ( 0.000000000000000000, 1.570796326794896558 ),
 .UNSPECIFIED. ) 
 CURVE ( )  GEOMETRIC_REPRESENTATION_ITEM ( )  RATIONAL_B_SPLINE_CURVE ( ( 1.000000000000000000, 0.8047378541243649375, 0.8047378541243649375, 1.000000000000000000 ) ) 
 REPRESENTATION_ITEM ( '' )  );
#5350 = CARTESIAN_POINT ( 'NONE',  ( 3.000000000000000000, 2.935248768560057897, -3.252606517456513302E-15 ) ) ;
#5351 = CARTESIAN_POINT ( 'NONE',  ( -43.93820948810023452, 0.000000000000000000, 0.000000000000000000 ) ) ;
#5352 = VERTEX_POINT ( 'NONE', #9457 ) ;
#5353 = CIRCLE ( 'NONE', #112, 4.000000000000007994 ) ;
#5354 = EDGE_LOOP ( 'NONE', ( #959, #3744 ) ) ;
#5355 = VECTOR ( 'NONE', #8036, 1000.000000000000000 ) ;
#5356 = ORIENTED_EDGE ( 'NONE', *, *, #10367, .T. ) ;
#5357 = VERTEX_POINT ( 'NONE', #5474 ) ;
#5358 = LINE ( 'NONE', #6957, #4193 ) ;
#5359 = DIRECTION ( 'NONE',  ( 0.000000000000000000, 0.000000000000000000, -1.000000000000000000 ) ) ;
#5360 = VECTOR ( 'NONE', #5861, 1000.000000000000000 ) ;
#5361 = DIRECTION ( 'NONE',  ( 0.000000000000000000, -0.000000000000000000, 1.000000000000000000 ) ) ;
#5362 = DIRECTION ( 'NONE',  ( 0.000000000000000000, 0.000000000000000000, 1.000000000000000000 ) ) ;
#5363 = CIRCLE ( 'NONE', #795, 10.00000000000000178 ) ;
#5364 = FACE_BOUND ( 'NONE', #8873, .T. ) ;
#5365 = ORIENTED_EDGE ( 'NONE', *, *, #5012, .T. ) ;
#5366 = LINE ( 'NONE', #9625, #6458 ) ;
#5367 = EDGE_CURVE ( 'NONE', #8901, #4776, #2191, .T. ) ;
#5368 = CLOSED_SHELL ( 'NONE', ( #7444, #2320, #487, #4815, #8507, #5190, #7409, #4414 ) ) ;
#5369 = CARTESIAN_POINT ( 'NONE',  ( -16.29350689640809691, -8.660287962196477451, 0.000000000000000000 ) ) ;
#5370 = CIRCLE ( 'NONE', #970, 7.499999999999998224 ) ;
#5371 = EDGE_CURVE ( 'NONE', #3083, #8958, #3896, .T. ) ;
#5372 = ORIENTED_EDGE ( 'NONE', *, *, #556, .T. ) ;
#5373 = AXIS2_PLACEMENT_3D ( 'NONE', #4138, #8216, #8110 ) ;
#5374 = CYLINDRICAL_SURFACE ( 'NONE', #6553, 5.000000000000007994 ) ;
#5375 = CARTESIAN_POINT ( 'NONE',  ( 3.000000000000000000, -2.935248768560057009, 4.770489558936219510E-15 ) ) ;
#5376 = FACE_OUTER_BOUND ( 'NONE', #1705, .T. ) ;
#5377 = EDGE_LOOP ( 'NONE', ( #7066, #8281 ) ) ;
#5378 = DIRECTION ( 'NONE',  ( 0.000000000000000000, 0.000000000000000000, -1.000000000000000000 ) ) ;
#5379 = ORIENTED_EDGE ( 'NONE', *, *, #1140, .F. ) ;
#5380 = SHAPE_DEFINITION_REPRESENTATION ( #2975, #6905 ) ;
#5381 = EDGE_CURVE ( 'NONE', #5111, #6261, #2814, .T. ) ;
#5382 = EDGE_LOOP ( 'NONE', ( #3205, #4639, #5523, #1008 ) ) ;
#5383 = AXIS2_PLACEMENT_3D ( 'NONE', #6403, #2375, #5607 ) ;
#5384 = CARTESIAN_POINT ( 'NONE',  ( -136.9408974318168646, 256.2777510384881339, 1.065925755226830171E-15 ) ) ;
#5385 = ORIENTED_EDGE ( 'NONE', *, *, #6575, .T. ) ;
#5386 = AXIS2_PLACEMENT_3D ( 'NONE', #6389, #9642, #2318 ) ;
#5387 = ORIENTED_EDGE ( 'NONE', *, *, #8448, .T. ) ;
#5388 = DIRECTION ( 'NONE',  ( 1.000000000000000000, 0.000000000000000000, 0.000000000000000000 ) ) ;
#5389 = CYLINDRICAL_SURFACE ( 'NONE', #7573, 7.999999999999989342 ) ;
#5390 = CARTESIAN_POINT ( 'NONE',  ( -18.34874108452141783, -140.1746510883711778, 7.212905963064383918 ) ) ;
#5391 = DIRECTION ( 'NONE',  ( 0.000000000000000000, 0.000000000000000000, -1.000000000000000000 ) ) ;
#5392 = DIRECTION ( 'NONE',  ( 0.000000000000000000, -1.000000000000000000, 0.000000000000000000 ) ) ;
#5393 = CARTESIAN_POINT ( 'NONE',  ( 26.62179802177712062, -135.1457019118818721, 49.99999999999997868 ) ) ;
#5394 = TOROIDAL_SURFACE ( 'NONE', #8783, 16.62298474266377468, 9.050254677131421843 ) ;
#5395 = ADVANCED_FACE ( 'NONE', ( #5521 ), #1505, .T. ) ;
#5396 = ORIENTED_EDGE ( 'NONE', *, *, #6053, .F. ) ;
#5397 = EDGE_CURVE ( 'NONE', #3840, #3587, #499, .T. ) ;
#5398 = CYLINDRICAL_SURFACE ( 'NONE', #2138, 3.999999999999989786 ) ;
#5399 = ADVANCED_FACE ( 'NONE', ( #6963 ), #6269, .F. ) ;
#5400 = ORIENTED_EDGE ( 'NONE', *, *, #10477, .T. ) ;
#5401 = DIRECTION ( 'NONE',  ( 1.000000000000000000, -0.000000000000000000, -0.000000000000000000 ) ) ;
#5402 = CARTESIAN_POINT ( 'NONE',  ( -18.34874108452141783, -140.1746510883711778, -97.78965767959371647 ) ) ;
#5403 = AXIS2_PLACEMENT_3D ( 'NONE', #5658, #106, #4964 ) ;
#5404 = DIRECTION ( 'NONE',  ( -1.000000000000000000, -0.000000000000000000, -0.000000000000000000 ) ) ;
#5405 = CARTESIAN_POINT ( 'NONE',  ( -2.293506896408097795, 120.5696653505793705, 20.00000000000000711 ) ) ;
#5406 = DIRECTION ( 'NONE',  ( -0.000000000000000000, 1.000000000000000000, -0.000000000000000000 ) ) ;
#5407 = ORIENTED_EDGE ( 'NONE', *, *, #8630, .F. ) ;
#5408 = ORIENTED_EDGE ( 'NONE', *, *, #500, .T. ) ;
#5409 = EDGE_CURVE ( 'NONE', #6945, #3453, #9250, .T. ) ;
#5410 = ADVANCED_FACE ( 'NONE', ( #10357 ), #5310, .F. ) ;
#5411 = EDGE_CURVE ( 'NONE', #5226, #2102, #1289, .T. ) ;
#5412 = ORIENTED_EDGE ( 'NONE', *, *, #6698, .F. ) ;
#5413 = ORIENTED_EDGE ( 'NONE', *, *, #5202, .F. ) ;
#5414 = CARTESIAN_POINT ( 'NONE',  ( -166.0794662972351716, 270.8019239353934040, 0.000000000000000000 ) ) ;
#5415 = CARTESIAN_POINT ( 'NONE',  ( 23.15769640663936713, -133.1457019118818721, 49.99999999999997868 ) ) ;
#5416 = CARTESIAN_POINT ( 'NONE',  ( -8.793506896408096907, 120.5289575273812233, 7.750000000000020428 ) ) ;
#5417 = DIRECTION ( 'NONE',  ( 1.000000000000000000, 0.000000000000000000, 0.000000000000000000 ) ) ;
#5418 = DIRECTION ( 'NONE',  ( -1.000000000000000000, 0.000000000000000000, 0.000000000000000000 ) ) ;
#5419 = ORIENTED_EDGE ( 'NONE', *, *, #3182, .T. ) ;
#5420 = CARTESIAN_POINT ( 'NONE',  ( -51.88626362769066702, 173.3644333388386656, 4.898587196589412829E-16 ) ) ;
#5421 = ADVANCED_FACE ( 'NONE', ( #2244 ), #8706, .T. ) ;
#5422 = ORIENTED_EDGE ( 'NONE', *, *, #9951, .T. ) ;
#5423 = CARTESIAN_POINT ( 'NONE',  ( -2.293506896408097795, 37.08684478514406635, 15.00000000000000355 ) ) ;
#5424 = PRODUCT ( 'MAS-316', 'MAS-316', '', ( #6175 ) ) ;
#5425 = EDGE_CURVE ( 'NONE', #8668, #7191, #6217, .T. ) ;
#5426 = CARTESIAN_POINT ( 'NONE',  ( -18.34874108452141783, -140.1746510883711778, -50.00000000000002132 ) ) ;
#5427 = DIRECTION ( 'NONE',  ( 1.000000000000000000, 0.000000000000000000, 0.000000000000000000 ) ) ;
#5428 = CARTESIAN_POINT ( 'NONE',  ( -7.293506896408097795, 72.56966535057935630, -20.00000000000001066 ) ) ;
#5429 = VERTEX_POINT ( 'NONE', #9400 ) ;
#5430 = CIRCLE ( 'NONE', #700, 31.75575292317714471 ) ;
#5431 = LINE ( 'NONE', #10370, #8502 ) ;
#5432 = ADVANCED_BREP_SHAPE_REPRESENTATION ( '', ( #9943, #4601 ), #409 ) ;
#5433 = ORIENTED_EDGE ( 'NONE', *, *, #9503, .F. ) ;
#5434 = ORIENTED_EDGE ( 'NONE', *, *, #3042, .T. ) ;
#5435 = DIRECTION ( 'NONE',  ( -0.7071067811863512853, 8.659560562357336419E-17, -0.7071067811867437491 ) ) ;
#5436 = ORIENTED_EDGE ( 'NONE', *, *, #10263, .T. ) ;
#5437 = AXIS2_PLACEMENT_3D ( 'NONE', #6431, #924, #9033 ) ;
#5438 = AXIS2_PLACEMENT_3D ( 'NONE', #9311, #1145, #1248 ) ;
#5439 = VERTEX_POINT ( 'NONE', #2134 ) ;
#5440 = DIRECTION ( 'NONE',  ( -0.000000000000000000, 1.000000000000000000, -0.000000000000000000 ) ) ;
#5441 = ADVANCED_FACE ( 'NONE', ( #4680, #5364 ), #8603, .F. ) ;
#5442 = CARTESIAN_POINT ( 'NONE',  ( -56.34457570605425758, 137.0132282531173473, -3.999999999999976019 ) ) ;
#5443 = CARTESIAN_POINT ( 'NONE',  ( 6.756858349438874534, 146.7073643690755773, 25.00000000000000000 ) ) ;
#5444 = PLANE ( 'NONE',  #3986 ) ;
#5445 = CARTESIAN_POINT ( 'NONE',  ( 4.856471286862176662, 147.5696653505793279, -25.00000000000002132 ) ) ;
#5446 = DIRECTION ( 'NONE',  ( -0.000000000000000000, -1.000000000000000000, -0.000000000000000000 ) ) ;
#5447 = CIRCLE ( 'NONE', #5106, 10.00000000000000178 ) ;
#5448 = VECTOR ( 'NONE', #7856, 1000.000000000000000 ) ;
#5449 = ORIENTED_EDGE ( 'NONE', *, *, #2399, .T. ) ;
#5450 = DIRECTION ( 'NONE',  ( 1.000000000000000000, -0.000000000000000000, 8.379529552680125332E-16 ) ) ;
#5451 = ORIENTED_EDGE ( 'NONE', *, *, #9615, .T. ) ;
#5452 = DIRECTION ( 'NONE',  ( -0.7431448254773957984, 0.6691306063588565722, -0.000000000000000000 ) ) ;
#5453 = DIRECTION ( 'NONE',  ( 1.000000000000000000, 0.000000000000000000, -0.000000000000000000 ) ) ;
#5454 = AXIS2_PLACEMENT_3D ( 'NONE', #4337, #6131, #6720 ) ;
#5455 = ORIENTED_EDGE ( 'NONE', *, *, #4551, .F. ) ;
#5456 = CIRCLE ( 'NONE', #6304, 2.000000000000001776 ) ;
#5457 = LINE ( 'NONE', #7058, #4460 ) ;
#5458 = EDGE_CURVE ( 'NONE', #8005, #9088, #4625, .T. ) ;
#5459 = CARTESIAN_POINT ( 'NONE',  ( -23.79350689640809335, 76.32362273389503571, 7.750000000000020428 ) ) ;
#5460 = DIRECTION ( 'NONE',  ( 1.137729606058012035E-16, 0.000000000000000000, 1.000000000000000000 ) ) ;
#5461 = VERTEX_POINT ( 'NONE', #6371 ) ;
#5462 = ORIENTED_EDGE ( 'NONE', *, *, #9293, .T. ) ;
#5463 = AXIS2_PLACEMENT_3D ( 'NONE', #9566, #9669, #12 ) ;
#5464 = CIRCLE ( 'NONE', #9515, 4.000000000000000000 ) ;
#5465 = ORIENTED_EDGE ( 'NONE', *, *, #6506, .T. ) ;
#5466 = VERTEX_POINT ( 'NONE', #3239 ) ;
#5467 = FACE_BOUND ( 'NONE', #3191, .T. ) ;
#5468 = CARTESIAN_POINT ( 'NONE',  ( -24.29350689640808625, 140.5696653505793563, -20.00000000000000711 ) ) ;
#5469 = CARTESIAN_POINT ( 'NONE',  ( -30.29350689640809335, 2.445795361565304815E-15, -20.00000000000002132 ) ) ;
#5470 = CARTESIAN_POINT ( 'NONE',  ( -16.29350689640810756, 140.5696653505793563, 20.00000000000002132 ) ) ;
#5471 = EDGE_CURVE ( 'NONE', #510, #3403, #8862, .T. ) ;
#5472 = ADVANCED_FACE ( 'NONE', ( #70 ), #8115, .F. ) ;
#5473 = EDGE_CURVE ( 'NONE', #4869, #5603, #2135, .T. ) ;
#5474 = CARTESIAN_POINT ( 'NONE',  ( 23.15769640663939910, -115.1457019118818863, -48.00000000000002132 ) ) ;
#5475 = DIRECTION ( 'NONE',  ( 1.000000000000000000, 0.000000000000000000, 0.000000000000000000 ) ) ;
#5476 = ORIENTED_EDGE ( 'NONE', *, *, #6543, .T. ) ;
#5477 = DIRECTION ( 'NONE',  ( -0.6691306063588574604, -0.7431448254773949103, 0.000000000000000000 ) ) ;
#5478 = EDGE_CURVE ( 'NONE', #9437, #1028, #853, .T. ) ;
#5479 = CARTESIAN_POINT ( 'NONE',  ( 14.70649310359190309, 80.56966535057935630, -16.00000000000000711 ) ) ;
#5480 = CARTESIAN_POINT ( 'NONE',  ( 53.40242741783141156, 52.77167129626698028, -25.00000000000000355 ) ) ;
#5481 = CARTESIAN_POINT ( 'NONE',  ( 3.000000000000000000, -2.935248768560057009, 4.770489558936219510E-15 ) ) ;
#5482 = VECTOR ( 'NONE', #4116, 1000.000000000000000 ) ;
#5483 = ORIENTED_EDGE ( 'NONE', *, *, #10298, .F. ) ;
#5484 = DIRECTION ( 'NONE',  ( 0.000000000000000000, 0.000000000000000000, 1.000000000000000000 ) ) ;
#5485 = PRODUCT_CONTEXT ( 'NONE', #7680, 'mechanical' ) ;
#5486 = EDGE_LOOP ( 'NONE', ( #8671, #2967, #5083, #4199, #1824 ) ) ;
#5487 = DIRECTION ( 'NONE',  ( -0.000000000000000000, -0.000000000000000000, 1.000000000000000000 ) ) ;
#5488 = EDGE_LOOP ( 'NONE', ( #747, #8066 ) ) ;
#5489 = AXIS2_PLACEMENT_3D ( 'NONE', #2564, #4784, #5793 ) ;
#5490 = VERTEX_POINT ( 'NONE', #7224 ) ;
#5491 = DIRECTION ( 'NONE',  ( 0.000000000000000000, 1.000000000000000000, 0.000000000000000000 ) ) ;
#5492 = CARTESIAN_POINT ( 'NONE',  ( -39.65624476065125492, 3.117691453623999909, -1.799999999999972955 ) ) ;
#5493 = DIRECTION ( 'NONE',  ( 0.000000000000000000, 0.000000000000000000, -1.000000000000000000 ) ) ;
#5494 = CARTESIAN_POINT ( 'NONE',  ( 39.99999999999997158, -135.1457019118818721, 44.02499999999997726 ) ) ;
#5495 = FACE_OUTER_BOUND ( 'NONE', #9273, .T. ) ;
#5496 = DIRECTION ( 'NONE',  ( 0.000000000000000000, 1.000000000000000000, 0.000000000000000000 ) ) ;
#5497 = FACE_OUTER_BOUND ( 'NONE', #513, .T. ) ;
#5498 = VECTOR ( 'NONE', #5406, 1000.000000000000000 ) ;
#5499 = EDGE_CURVE ( 'NONE', #7087, #10167, #2822, .T. ) ;
#5500 = ORIENTED_EDGE ( 'NONE', *, *, #4093, .F. ) ;
#5501 = CIRCLE ( 'NONE', #930, 2.000000000000001776 ) ;
#5502 = DIRECTION ( 'NONE',  ( -0.6691306063588566833, -0.7431448254773955764, 0.000000000000000000 ) ) ;
#5503 = ORIENTED_EDGE ( 'NONE', *, *, #1846, .T. ) ;
#5504 = FACE_OUTER_BOUND ( 'NONE', #5036, .T. ) ;
#5505 =( NAMED_UNIT ( * ) SI_UNIT ( $, .STERADIAN. ) SOLID_ANGLE_UNIT ( ) );
#5506 = CARTESIAN_POINT ( 'NONE',  ( -27.15769640663939555, -117.1457019118819005, -25.15769640663944173 ) ) ;
#5507 = FACE_OUTER_BOUND ( 'NONE', #3093, .T. ) ;
#5508 = AXIS2_PLACEMENT_3D ( 'NONE', #3917, #6291, #8832 ) ;
#5509 = VERTEX_POINT ( 'NONE', #960 ) ;
#5510 = ORIENTED_EDGE ( 'NONE', *, *, #8446, .F. ) ;
#5511 = VECTOR ( 'NONE', #5046, 1000.000000000000000 ) ;
#5512 = PRODUCT_DEFINITION_SHAPE ( 'NONE', 'NONE',  #10481 ) ;
#5513 = EDGE_CURVE ( 'NONE', #1149, #4585, #9431, .T. ) ;
#5514 = CIRCLE ( 'NONE', #6874, 0.4000000000000000222 ) ;
#5515 = ORIENTED_EDGE ( 'NONE', *, *, #803, .F. ) ;
#5516 = CARTESIAN_POINT ( 'NONE',  ( -50.00000000000002842, -133.6309146189979344, -23.64292728780891650 ) ) ;
#5517 = CARTESIAN_POINT ( 'NONE',  ( -27.15769640663939555, -117.1457019118819005, -27.15769640663944173 ) ) ;
#5518 = CARTESIAN_POINT ( 'NONE',  ( -56.36957570605427748, 150.5696653505793563, 10.90000000000000036 ) ) ;
#5519 = FACE_OUTER_BOUND ( 'NONE', #4352, .T. ) ;
#5520 = AXIS2_PLACEMENT_3D ( 'NONE', #2169, #8632, #583 ) ;
#5521 = FACE_OUTER_BOUND ( 'NONE', #8643, .T. ) ;
#5522 = AXIS2_PLACEMENT_3D ( 'NONE', #3784, #8551, #9512 ) ;
#5523 = ORIENTED_EDGE ( 'NONE', *, *, #171, .T. ) ;
#5524 = DIRECTION ( 'NONE',  ( -1.000000000000000000, -0.000000000000000000, -0.000000000000000000 ) ) ;
#5525 = ADVANCED_FACE ( 'NONE', ( #4825 ), #2552, .F. ) ;
#5526 = CIRCLE ( 'NONE', #10287, 3.999999999999989786 ) ;
#5527 = EDGE_CURVE ( 'NONE', #2815, #7140, #7274, .T. ) ;
#5528 = VERTEX_POINT ( 'NONE', #3141 ) ;
#5529 = EDGE_CURVE ( 'NONE', #9125, #4228, #10282, .T. ) ;
#5530 = CARTESIAN_POINT ( 'NONE',  ( -27.15769640663939555, -115.1457019118818863, -23.15769640663943463 ) ) ;
#5531 = UNCERTAINTY_MEASURE_WITH_UNIT (LENGTH_MEASURE( 1.000000000000000082E-05 ), #7330, 'distance_accuracy_value', 'NONE');
#5532 = AXIS2_PLACEMENT_3D ( 'NONE', #5576, #5726, #4924 ) ;
#5533 = AXIS2_PLACEMENT_3D ( 'NONE', #7870, #3903, #3793 ) ;
#5534 = DIRECTION ( 'NONE',  ( -1.000000000000000000, 0.000000000000000000, 0.000000000000000000 ) ) ;
#5535 = FACE_OUTER_BOUND ( 'NONE', #5177, .T. ) ;
#5536 = LINE ( 'NONE', #1463, #8556 ) ;
#5537 = AXIS2_PLACEMENT_3D ( 'NONE', #7080, #7230, #6330 ) ;
#5538 = ORIENTED_EDGE ( 'NONE', *, *, #7351, .F. ) ;
#5539 = CARTESIAN_POINT ( 'NONE',  ( 0.000000000000000000, -133.1457019118818721, 27.15769640663938489 ) ) ;
#5540 = VECTOR ( 'NONE', #6628, 1000.000000000000000 ) ;
#5541 = SHAPE_DEFINITION_REPRESENTATION ( #7796, #286 ) ;
#5543 = EDGE_CURVE ( 'NONE', #4361, #39, #4981, .T. ) ;
#5542 = VERTEX_POINT ( 'NONE', #1756 ) ;
#5544 = EDGE_CURVE ( 'NONE', #2948, #6365, #4880, .T. ) ;
#5545 = CARTESIAN_POINT ( 'NONE',  ( -142.3328939341254795, 249.4204141414382434, 0.000000000000000000 ) ) ;
#5546 = EDGE_LOOP ( 'NONE', ( #5571, #4979, #8645, #9724 ) ) ;
#5547 = VECTOR ( 'NONE', #5995, 1000.000000000000000 ) ;
#5548 = ORIENTED_EDGE ( 'NONE', *, *, #8300, .F. ) ;
#5549 = DIRECTION ( 'NONE',  ( -0.7431448254773957984, 0.6691306063588565722, -0.000000000000000000 ) ) ;
#5550 = DIRECTION ( 'NONE',  ( 8.379529552680124346E-16, 0.000000000000000000, -1.000000000000000000 ) ) ;
#5551 = FACE_OUTER_BOUND ( 'NONE', #8697, .T. ) ;
#5552 = DIRECTION ( 'NONE',  ( 0.000000000000000000, 0.000000000000000000, -1.000000000000000000 ) ) ;
#5553 = CARTESIAN_POINT ( 'NONE',  ( -50.00000000000001421, -145.1457019118819005, -40.00000000000002132 ) ) ;
#5554 = DIRECTION ( 'NONE',  ( 0.000000000000000000, 1.000000000000000000, 0.000000000000000000 ) ) ;
#5555 = CIRCLE ( 'NONE', #5383, 20.00000000000000000 ) ;
#5556 = VERTEX_POINT ( 'NONE', #2446 ) ;
#5557 = EDGE_CURVE ( 'NONE', #4542, #4517, #787, .T. ) ;
#5558 = LINE ( 'NONE', #9699, #8578 ) ;
#5559 = CIRCLE ( 'NONE', #149, 7.525240063345735919 ) ;
#5560 = ORIENTED_EDGE ( 'NONE', *, *, #6341, .F. ) ;
#5561 = CARTESIAN_POINT ( 'NONE',  ( -30.29350689640809335, 150.5696653505793563, -20.00000000000000355 ) ) ;
#5562 = VECTOR ( 'NONE', #5970, 1000.000000000000000 ) ;
#5563 = DIRECTION ( 'NONE',  ( 0.000000000000000000, -1.000000000000000000, 0.000000000000000000 ) ) ;
#5564 = EDGE_CURVE ( 'NONE', #8380, #477, #7225, .T. ) ;
#5565 = ADVANCED_FACE ( 'NONE', ( #2347 ), #2499, .T. ) ;
#5566 = DIRECTION ( 'NONE',  ( -1.000000000000000000, -0.000000000000000000, -0.000000000000000000 ) ) ;
#5567 = SPHERICAL_SURFACE ( 'NONE', #2450, 2.000000000000000000 ) ;
#5568 = AXIS2_PLACEMENT_3D ( 'NONE', #7609, #3791, #4476 ) ;
#5569 = ORIENTED_EDGE ( 'NONE', *, *, #4710, .T. ) ;
#5570 = ORIENTED_EDGE ( 'NONE', *, *, #6249, .T. ) ;
#5571 = ORIENTED_EDGE ( 'NONE', *, *, #2882, .F. ) ;
#5572 = CIRCLE ( 'NONE', #8960, 5.000000000000000888 ) ;
#5573 = DIRECTION ( 'NONE',  ( -1.000000000000000000, -0.000000000000000000, -0.000000000000000000 ) ) ;
#5574 = CARTESIAN_POINT ( 'NONE',  ( -40.33539666817951996, -0.09126465619898782577, 4.000000000000000888 ) ) ;
#5575 = CARTESIAN_POINT ( 'NONE',  ( -30.29350689640809335, 120.5696653505793705, 20.00000000000000711 ) ) ;
#5576 = CARTESIAN_POINT ( 'NONE',  ( -31.74999999999995737, 0.000000000000000000, 0.000000000000000000 ) ) ;
#5577 = VERTEX_POINT ( 'NONE', #8166 ) ;
#5578 = AXIS2_PLACEMENT_3D ( 'NONE', #7572, #2693, #5920 ) ;
#5579 = DIRECTION ( 'NONE',  ( -1.000000000000000000, 0.000000000000000000, 0.000000000000000000 ) ) ;
#5580 = EDGE_LOOP ( 'NONE', ( #1226, #3921, #1108, #10450 ) ) ;
#5581 = ORIENTED_EDGE ( 'NONE', *, *, #8183, .T. ) ;
#5582 = CARTESIAN_POINT ( 'NONE',  ( -97.04168628513711781, 208.6400276031560566, 0.000000000000000000 ) ) ;
#5583 = CARTESIAN_POINT ( 'NONE',  ( 0.000000000000000000, 1.467624384280033167, 2.541999999999999371 ) ) ;
#5584 = ADVANCED_FACE ( 'NONE', ( #8809 ), #1296, .F. ) ;
#5585 = DIRECTION ( 'NONE',  ( 0.000000000000000000, 0.000000000000000000, -1.000000000000000000 ) ) ;
#5586 = ORIENTED_EDGE ( 'NONE', *, *, #3642, .F. ) ;
#5587 = DIRECTION ( 'NONE',  ( 0.6585271261848804070, -0.7525569905852197428, -0.000000000000000000 ) ) ;
#5588 = CONTEXT_DEPENDENT_SHAPE_REPRESENTATION ( #1858, #4835 ) ;
#5589 = VERTEX_POINT ( 'NONE', #909 ) ;
#5590 = CARTESIAN_POINT ( 'NONE',  ( -20.29350689640809691, 140.5696653505793563, -10.98204862120179826 ) ) ;
#5591 = ORIENTED_EDGE ( 'NONE', *, *, #3884, .F. ) ;
#5592 = ORIENTED_EDGE ( 'NONE', *, *, #1198, .T. ) ;
#5593 = PLANE ( 'NONE',  #463 ) ;
#5594 = VECTOR ( 'NONE', #3918, 1000.000000000000000 ) ;
#5595 = CYLINDRICAL_SURFACE ( 'NONE', #5986, 10.00000000000000000 ) ;
#5596 = EDGE_CURVE ( 'NONE', #8325, #125, #1975, .T. ) ;
#5597 = EDGE_CURVE ( 'NONE', #1304, #8738, #6685, .T. ) ;
#5598 = CYLINDRICAL_SURFACE ( 'NONE', #3475, 4.000000000000000000 ) ;
#5599 = EDGE_CURVE ( 'NONE', #8767, #1043, #9124, .T. ) ;
#5600 = DIRECTION ( 'NONE',  ( 1.000000000000000000, 0.000000000000000000, -0.000000000000000000 ) ) ;
#5601 = CARTESIAN_POINT ( 'NONE',  ( -16.29350689640809691, -115.1457019118818863, 0.000000000000000000 ) ) ;
#5602 = PRODUCT_DEFINITION_SHAPE ( 'NONE', 'NONE',  #10482 ) ;
#5603 = VERTEX_POINT ( 'NONE', #7638 ) ;
#5604 = DIRECTION ( 'NONE',  ( 0.000000000000000000, 0.000000000000000000, 1.000000000000000000 ) ) ;
#5605 = AXIS2_PLACEMENT_3D ( 'NONE', #1091, #2781, #2836 ) ;
#5606 = ORIENTED_EDGE ( 'NONE', *, *, #10408, .F. ) ;
#5607 = DIRECTION ( 'NONE',  ( 1.000000000000000000, -1.387778780781445676E-15, -1.301042606982605321E-16 ) ) ;
#5608 = LINE ( 'NONE', #7901, #5806 ) ;
#5609 = CARTESIAN_POINT ( 'NONE',  ( -11.29350689640809158, 105.5289575273812233, 10.90000000000000036 ) ) ;
#5610 = VECTOR ( 'NONE', #3786, 1000.000000000000000 ) ;
#5611 = EDGE_CURVE ( 'NONE', #9925, #6151, #7564, .T. ) ;
#5612 = CARTESIAN_POINT ( 'NONE',  ( -38.19229777560033057, 37.08684478514405214, 12.50000000000000000 ) ) ;
#5613 = AXIS2_PLACEMENT_3D ( 'NONE', #7428, #7474, #173 ) ;
#5614 = ORIENTED_EDGE ( 'NONE', *, *, #9010, .F. ) ;
#5615 = ORIENTED_EDGE ( 'NONE', *, *, #6086, .F. ) ;
#5616 = AXIS2_PLACEMENT_3D ( 'NONE', #1207, #4439, #8520 ) ;
#5617 = VERTEX_POINT ( 'NONE', #5393 ) ;
#5618 = CIRCLE ( 'NONE', #8836, 3.297986701801175258 ) ;
#5619 = FACE_OUTER_BOUND ( 'NONE', #684, .T. ) ;
#5620 = CARTESIAN_POINT ( 'NONE',  ( 24.41866285951198634, -134.3099192498708874, 49.99999999999998579 ) ) ;
#5621 = CARTESIAN_POINT ( 'NONE',  ( 23.15769640663940265, -115.1457019118818863, -50.00000000000002132 ) ) ;
#5622 = LINE ( 'NONE', #7220, #7665 ) ;
#5623 = ORIENTED_EDGE ( 'NONE', *, *, #6959, .T. ) ;
#5624 = DIRECTION ( 'NONE',  ( 0.000000000000000000, 0.000000000000000000, 1.000000000000000000 ) ) ;
#5625 = ORIENTED_EDGE ( 'NONE', *, *, #274, .F. ) ;
#5626 = AXIS2_PLACEMENT_3D ( 'NONE', #4996, #4840, #8079 ) ;
#5627 = LINE ( 'NONE', #3404, #2185 ) ;
#5628 = CIRCLE ( 'NONE', #2411, 26.75575292317714116 ) ;
#5629 = EDGE_CURVE ( 'NONE', #9180, #1816, #5020, .T. ) ;
#5630 = VERTEX_POINT ( 'NONE', #2605 ) ;
#5631 = LINE ( 'NONE', #4687, #1986 ) ;
#5632 = AXIS2_PLACEMENT_3D ( 'NONE', #3929, #7207, #1435 ) ;
#5633 = CARTESIAN_POINT ( 'NONE',  ( 3.000000000000000000, 3.380207847158609940E-15, 2.542000000000001592 ) ) ;
#5634 = DIRECTION ( 'NONE',  ( 0.000000000000000000, 0.000000000000000000, -1.000000000000000000 ) ) ;
#5635 = EDGE_LOOP ( 'NONE', ( #5113, #3181, #4344, #3407, #2519 ) ) ;
#5636 = DIRECTION ( 'NONE',  ( 1.000000000000000000, 0.000000000000000000, 0.000000000000000000 ) ) ;
#5637 = AXIS2_PLACEMENT_3D ( 'NONE', #8469, #10172, #8364 ) ;
#5638 = ITEM_DEFINED_TRANSFORMATION ( 'NONE', 'NONE', #8870,  #4601 ) ;
#5639 = EDGE_LOOP ( 'NONE', ( #1307, #9533, #7630, #8459 ) ) ;
#5640 = CARTESIAN_POINT ( 'NONE',  ( 4.856471286862176662, 145.0444252872335937, -12.49999999999999289 ) ) ;
#5641 = EDGE_CURVE ( 'NONE', #9162, #4377, #7927, .T. ) ;
#5642 = ORIENTED_EDGE ( 'NONE', *, *, #7364, .T. ) ;
#5643 = ORIENTED_EDGE ( 'NONE', *, *, #6007, .T. ) ;
#5644 = VECTOR ( 'NONE', #2680, 1000.000000000000000 ) ;
#5645 = FACE_BOUND ( 'NONE', #5666, .T. ) ;
#5646 = LINE ( 'NONE', #4222, #5482 ) ;
#5647 = CARTESIAN_POINT ( 'NONE',  ( 3.000000000000000000, 1.467624384280032501, 2.541999999999999371 ) ) ;
#5648 = CARTESIAN_POINT ( 'NONE',  ( -40.00000000000002842, -135.1457019118818721, 39.99999999999997868 ) ) ;
#5649 = VERTEX_POINT ( 'NONE', #1372 ) ;
#5650 = AXIS2_PLACEMENT_3D ( 'NONE', #3466, #7495, #1025 ) ;
#5651 = CARTESIAN_POINT ( 'NONE',  ( -27.15769640663940976, -117.1457019118819005, 23.15769640663938134 ) ) ;
#5652 = ADVANCED_FACE ( 'NONE', ( #9175 ), #6995, .T. ) ;
#5653 = EDGE_CURVE ( 'NONE', #5715, #852, #1015, .T. ) ;
#5654 = EDGE_CURVE ( 'NONE', #6648, #3816, #2650, .T. ) ;
#5655 = VERTEX_POINT ( 'NONE', #4408 ) ;
#5656 = CARTESIAN_POINT ( 'NONE',  ( -30.29350689640809335, 140.5696653505793563, 20.00000000000000355 ) ) ;
#5657 = CARTESIAN_POINT ( 'NONE',  ( -47.94539818030328604, 155.5289575273811522, 0.000000000000000000 ) ) ;
#5658 = CARTESIAN_POINT ( 'NONE',  ( 0.000000000000000000, 0.000000000000000000, 0.000000000000000000 ) ) ;
#5659 = CARTESIAN_POINT ( 'NONE',  ( -30.29350689640809335, 72.56966535057935630, -20.00000000000001066 ) ) ;
#5660 = CARTESIAN_POINT ( 'NONE',  ( 14.70649310359190309, 80.56966535057935630, 24.00000000000000711 ) ) ;
#5661 = CARTESIAN_POINT ( 'NONE',  ( 37.22511195853869026, -145.1457019118819005, 30.00000000000000355 ) ) ;
#5662 = ORIENTED_EDGE ( 'NONE', *, *, #2486, .F. ) ;
#5663 = ORIENTED_EDGE ( 'NONE', *, *, #1490, .F. ) ;
#5664 = CIRCLE ( 'NONE', #8720, 7.572730065532343069 ) ;
#5665 = ORIENTED_EDGE ( 'NONE', *, *, #8390, .T. ) ;
#5666 = EDGE_LOOP ( 'NONE', ( #7500, #2457 ) ) ;
#5667 = EDGE_CURVE ( 'NONE', #3031, #6869, #4353, .T. ) ;
#5668 = PLANE ( 'NONE',  #7751 ) ;
#5669 = DIRECTION ( 'NONE',  ( 0.000000000000000000, 0.000000000000000000, 1.000000000000000000 ) ) ;
#5670 = FACE_OUTER_BOUND ( 'NONE', #6688, .T. ) ;
#5671 = VERTEX_POINT ( 'NONE', #7590 ) ;
#5672 = CARTESIAN_POINT ( 'NONE',  ( -7.293506896408097795, 2.445795361565304815E-15, 20.00000000000002132 ) ) ;
#5673 = ORIENTED_EDGE ( 'NONE', *, *, #10408, .T. ) ;
#5674 = CARTESIAN_POINT ( 'NONE',  ( -0.8557715602033003632, 3.117691453623996356, -1.799999999999970957 ) ) ;
#5675 = VECTOR ( 'NONE', #1730, 1000.000000000000000 ) ;
#5676 = ORIENTED_EDGE ( 'NONE', *, *, #4668, .T. ) ;
#5677 = PRODUCT_DEFINITION_CONTEXT ( 'detailed design', #5107, 'design' ) ;
#5678 = DIRECTION ( 'NONE',  ( 0.000000000000000000, 0.000000000000000000, -1.000000000000000000 ) ) ;
#5679 = VECTOR ( 'NONE', #8728, 1000.000000000000000 ) ;
#5680 = LINE ( 'NONE', #3057, #45 ) ;
#5681 = PRODUCT ( 'groove pin 01_iso_ISO 8739-M8x45-St', 'groove pin 01_iso_ISO 8739-M8x45-St', '', ( #5485 ) ) ;
#5682 = CARTESIAN_POINT ( 'NONE',  ( 17.97972049165455388, 17.84145331825995484, 30.00000000000000355 ) ) ;
#5683 = ADVANCED_FACE ( 'NONE', ( #1911 ), #5830, .T. ) ;
#5684 = LINE ( 'NONE', #2513, #780 ) ;
#5685 = ORIENTED_EDGE ( 'NONE', *, *, #8347, .F. ) ;
#5686 = CYLINDRICAL_SURFACE ( 'NONE', #5626, 20.00000000000000000 ) ;
#5687 = VECTOR ( 'NONE', #7802, 1000.000000000000000 ) ;
#5688 = SHAPE_DEFINITION_REPRESENTATION ( #9597, #1081 ) ;
#5689 = VERTEX_POINT ( 'NONE', #281 ) ;
#5690 = CARTESIAN_POINT ( 'NONE',  ( -16.26850689640809833, 140.5696653505793563, 10.90000000000000036 ) ) ;
#5691 = ORIENTED_EDGE ( 'NONE', *, *, #1787, .T. ) ;
#5692 = CIRCLE ( 'NONE', #6375, 3.999999999999998668 ) ;
#5693 = FACE_OUTER_BOUND ( 'NONE', #10033, .T. ) ;
#5694 = DIRECTION ( 'NONE',  ( 0.000000000000000000, -1.000000000000000000, 0.000000000000000000 ) ) ;
#5695 = CARTESIAN_POINT ( 'NONE',  ( -36.36957570605426326, 137.0132282531173473, -4.000000000000003553 ) ) ;
#5696 = DIRECTION ( 'NONE',  ( 0.000000000000000000, 0.000000000000000000, -1.000000000000000000 ) ) ;
#5697 = VECTOR ( 'NONE', #1988, 1000.000000000000000 ) ;
#5698 = DIRECTION ( 'NONE',  ( -1.734723475976805517E-15, 1.000000000000000000, 0.000000000000000000 ) ) ;
#5699 = ADVANCED_FACE ( 'NONE', ( #5886 ), #1174, .T. ) ;
#5700 = ORIENTED_EDGE ( 'NONE', *, *, #9826, .F. ) ;
#5701 = AXIS2_PLACEMENT_3D ( 'NONE', #10465, #4049, #2354 ) ;
#5702 = CARTESIAN_POINT ( 'NONE',  ( 37.22759939293836595, -133.1457019118818721, 25.15769640663938134 ) ) ;
#5703 = AXIS2_PLACEMENT_3D ( 'NONE', #9878, #6682, #1909 ) ;
#5704 = ORIENTED_EDGE ( 'NONE', *, *, #1026, .F. ) ;
#5705 = CARTESIAN_POINT ( 'NONE',  ( -7.293506896408097795, 120.5696653505793705, -20.00000000000000711 ) ) ;
#5706 = DIRECTION ( 'NONE',  ( -1.000000000000000000, 0.000000000000000000, 0.000000000000000000 ) ) ;
#5707 = FACE_OUTER_BOUND ( 'NONE', #7136, .T. ) ;
#5708 = CARTESIAN_POINT ( 'NONE',  ( -3.173844575093148990, 90.52895752738122326, 10.90000000000000036 ) ) ;
#5709 = CARTESIAN_POINT ( 'NONE',  ( -18.34874108452141783, -140.1746510883711778, -29.59847408863698703 ) ) ;
#5710 = AXIS2_PLACEMENT_3D ( 'NONE', #5150, #4362, #7598 ) ;
#5711 = DIRECTION ( 'NONE',  ( -0.000000000000000000, -0.000000000000000000, 1.000000000000000000 ) ) ;
#5712 = ORIENTED_EDGE ( 'NONE', *, *, #1052, .F. ) ;
#5713 = EDGE_CURVE ( 'NONE', #195, #1043, #124, .T. ) ;
#5714 = EDGE_CURVE ( 'NONE', #1670, #7639, #1812, .T. ) ;
#5715 = VERTEX_POINT ( 'NONE', #2962 ) ;
#5716 = ORIENTED_EDGE ( 'NONE', *, *, #5012, .F. ) ;
#5717 = VECTOR ( 'NONE', #3663, 1000.000000000000000 ) ;
#5718 = ORIENTED_EDGE ( 'NONE', *, *, #8696, .T. ) ;
#5719 = DIRECTION ( 'NONE',  ( -0.000000000000000000, 1.000000000000000000, 0.000000000000000000 ) ) ;
#5720 = DIRECTION ( 'NONE',  ( 0.000000000000000000, 0.000000000000000000, 1.000000000000000000 ) ) ;
#5721 = CIRCLE ( 'NONE', #4713, 3.999999999999999112 ) ;
#5722 = DIRECTION ( 'NONE',  ( 0.000000000000000000, 0.000000000000000000, 1.000000000000000000 ) ) ;
#5723 = CARTESIAN_POINT ( 'NONE',  ( -2.293506896408097795, 80.56966535057935630, -20.00000000000000711 ) ) ;
#5724 = ORIENTED_EDGE ( 'NONE', *, *, #4944, .T. ) ;
#5725 = EDGE_CURVE ( 'NONE', #9869, #5302, #8575, .T. ) ;
#5726 = DIRECTION ( 'NONE',  ( -1.000000000000000000, -0.000000000000000000, -0.000000000000000000 ) ) ;
#5727 = EDGE_CURVE ( 'NONE', #5912, #6555, #1065, .T. ) ;
#5728 = EDGE_CURVE ( 'NONE', #6514, #4464, #3156, .T. ) ;
#5729 = ORIENTED_EDGE ( 'NONE', *, *, #1530, .F. ) ;
#5730 = VERTEX_POINT ( 'NONE', #3919 ) ;
#5731 = ORIENTED_EDGE ( 'NONE', *, *, #10146, .F. ) ;
#5732 = DIRECTION ( 'NONE',  ( -0.000000000000000000, -0.000000000000000000, -1.000000000000000000 ) ) ;
#5733 = LINE ( 'NONE', #1712, #6526 ) ;
#5734 = CARTESIAN_POINT ( 'NONE',  ( 27.15769640663937068, -133.1457019118818721, 47.99999999999997868 ) ) ;
#5735 = AXIS2_PLACEMENT_3D ( 'NONE', #4908, #890, #4129 ) ;
#5736 = CARTESIAN_POINT ( 'NONE',  ( 38.19229777560031636, 37.08684478514405214, 12.50000000000000000 ) ) ;
#5737 = CARTESIAN_POINT ( 'NONE',  ( -2.293506896408101348, 147.5696653505793279, 30.00000000000000355 ) ) ;
#5738 = EDGE_CURVE ( 'NONE', #4025, #4617, #2274, .T. ) ;
#5739 = ORIENTED_EDGE ( 'NONE', *, *, #803, .T. ) ;
#5740 = DIRECTION ( 'NONE',  ( -1.000000000000000000, -0.000000000000000000, -0.000000000000000000 ) ) ;
#5741 = SHAPE_DEFINITION_REPRESENTATION ( #2124, #7587 ) ;
#5742 = VERTEX_POINT ( 'NONE', #1426 ) ;
#5743 = FACE_BOUND ( 'NONE', #5029, .T. ) ;
#5744 = EDGE_LOOP ( 'NONE', ( #10305, #3574, #6343, #5510 ) ) ;
#5745 = ADVANCED_FACE ( 'NONE', ( #5497 ), #7988, .F. ) ;
#5746 = SHAPE_REPRESENTATION_RELATIONSHIP ( 'NONE' , 'NONE' ,  #6561, #5055 ) ;
#5747 = SHAPE_REPRESENTATION ( 'Secondary Joint', ( #4601 ), #8362 ) ;
#5748 = FACE_OUTER_BOUND ( 'NONE', #7341, .T. ) ;
#5749 = CARTESIAN_POINT ( 'NONE',  ( 39.99999999999997158, -135.1457019118818721, 44.02499999999997726 ) ) ;
#5750 = DIRECTION ( 'NONE',  ( -0.000000000000000000, 1.000000000000000000, -0.000000000000000000 ) ) ;
#5751 = DIRECTION ( 'NONE',  ( 0.000000000000000000, 0.000000000000000000, 1.000000000000000000 ) ) ;
#5752 = ORIENTED_EDGE ( 'NONE', *, *, #9442, .T. ) ;
#5753 = DIRECTION ( 'NONE',  ( -1.000000000000000000, 0.000000000000000000, 0.000000000000000000 ) ) ;
#5754 = ADVANCED_FACE ( 'NONE', ( #4750 ), #1578, .T. ) ;
#5755 = VERTEX_POINT ( 'NONE', #2328 ) ;
#5756 = CARTESIAN_POINT ( 'NONE',  ( -16.29350689640809691, -8.660287962196477451, -4.999999999999995559 ) ) ;
#5757 = DIRECTION ( 'NONE',  ( -0.6691306063588565722, -0.7431448254773957984, 0.000000000000000000 ) ) ;
#5758 = FILL_AREA_STYLE_COLOUR ( '', #7269 ) ;
#5759 = FACE_OUTER_BOUND ( 'NONE', #9367, .T. ) ;
#5760 = CARTESIAN_POINT ( 'NONE',  ( -16.29350689640809691, 105.5289575273812233, -7.749999999999996447 ) ) ;
#5761 = CARTESIAN_POINT ( 'NONE',  ( -27.15769640663940976, -115.1457019118818863, 27.15769640663938489 ) ) ;
#5762 = ORIENTED_EDGE ( 'NONE', *, *, #1322, .F. ) ;
#5763 = CONICAL_SURFACE ( 'NONE', #527, 4.025000000000000355, 0.7853981633975870569 ) ;
#5764 = ORIENTED_EDGE ( 'NONE', *, *, #1961, .T. ) ;
#5765 = EDGE_LOOP ( 'NONE', ( #9663, #15, #1191, #2009 ) ) ;
#5766 = EDGE_LOOP ( 'NONE', ( #10071, #8819, #5718, #1123 ) ) ;
#5767 = EDGE_CURVE ( 'NONE', #8114, #2357, #4346, .T. ) ;
#5768 = CARTESIAN_POINT ( 'NONE',  ( 23.15769640663940265, -117.1457019118819005, -48.00000000000002132 ) ) ;
#5769 = DIRECTION ( 'NONE',  ( 0.000000000000000000, 0.000000000000000000, 1.000000000000000000 ) ) ;
#5770=STYLED_ITEM('',(#10525),#6821);
#5771 = CIRCLE ( 'NONE', #9518, 10.00000000000000178 ) ;
#5772 = LINE ( 'NONE', #6626, #4783 ) ;
#5773 = FACE_OUTER_BOUND ( 'NONE', #10137, .T. ) ;
#5774 = EDGE_LOOP ( 'NONE', ( #2196, #3725, #5160, #2208 ) ) ;
#5775 = CARTESIAN_POINT ( 'NONE',  ( 10.51964330236497602, 150.0000000000000000, 30.00000000000000355 ) ) ;
#5776 = ORIENTED_EDGE ( 'NONE', *, *, #5272, .T. ) ;
#5777 = CARTESIAN_POINT ( 'NONE',  ( -30.29350689640809335, 80.56966535057935630, 20.00000000000000711 ) ) ;
#5778 = VECTOR ( 'NONE', #4887, 1000.000000000000000 ) ;
#5779 = AXIS2_PLACEMENT_3D ( 'NONE', #3833, #2188, #4770 ) ;
#5780 = EDGE_LOOP ( 'NONE', ( #9142, #5341, #4895, #4971 ) ) ;
#5781 = UNCERTAINTY_MEASURE_WITH_UNIT (LENGTH_MEASURE( 1.000000000000000082E-05 ), #3234, 'distance_accuracy_value', 'NONE');
#5782 = ORIENTED_EDGE ( 'NONE', *, *, #6775, .T. ) ;
#5783 = VERTEX_POINT ( 'NONE', #3814 ) ;
#5784 = EDGE_CURVE ( 'NONE', #852, #2923, #1131, .T. ) ;
#5785 = CARTESIAN_POINT ( 'NONE',  ( 73.53765631853927687, 70.39106037767953694, 30.00000000000000355 ) ) ;
#5786 = EDGE_CURVE ( 'NONE', #6595, #7639, #9777, .T. ) ;
#5787 = CARTESIAN_POINT ( 'NONE',  ( -24.29350689640808625, 140.5696653505793563, 20.00000000000002132 ) ) ;
#5788 = EDGE_CURVE ( 'NONE', #6846, #1518, #1534, .T. ) ;
#5789 = LINE ( 'NONE', #9786, #9594 ) ;
#5790 = CARTESIAN_POINT ( 'NONE',  ( -40.00000000000002842, -145.1457019118819005, 35.99999999999999289 ) ) ;
#5791 = CIRCLE ( 'NONE', #2070, 7.728925574020642841 ) ;
#5792 = AXIS2_PLACEMENT_3D ( 'NONE', #6977, #4431, #2942 ) ;
#5793 = DIRECTION ( 'NONE',  ( -1.000000000000000000, 0.000000000000000000, -6.982941293900099513E-16 ) ) ;
#5794 = PLANE ( 'NONE',  #8744 ) ;
#5795 = ORIENTED_EDGE ( 'NONE', *, *, #6655, .T. ) ;
#5796 = DIRECTION ( 'NONE',  ( 0.000000000000000000, 0.000000000000000000, 1.000000000000000000 ) ) ;
#5797 = ITEM_DEFINED_TRANSFORMATION ( 'NONE', 'NONE', #2094,  #4601 ) ;
#5798 = ORIENTED_EDGE ( 'NONE', *, *, #9423, .F. ) ;
#5799 = CIRCLE ( 'NONE', #1056, 5.000000000000001776 ) ;
#5800 = CARTESIAN_POINT ( 'NONE',  ( -40.00000000000001421, -135.1457019118818721, -44.02500000000001990 ) ) ;
#5801 = ORIENTED_EDGE ( 'NONE', *, *, #2708, .F. ) ;
#5802 = ADVANCED_FACE ( 'NONE', ( #778 ), #8025, .F. ) ;
#5803 = FACE_OUTER_BOUND ( 'NONE', #1632, .T. ) ;
#5804 = CARTESIAN_POINT ( 'NONE',  ( 14.70649310359190309, 80.56966535057935630, 16.00000000000000711 ) ) ;
#5805 = DIRECTION ( 'NONE',  ( -0.000000000000000000, 1.000000000000000000, -0.000000000000000000 ) ) ;
#5806 = VECTOR ( 'NONE', #6406, 1000.000000000000000 ) ;
#5807 = CARTESIAN_POINT ( 'NONE',  ( -20.29350689640809691, 150.5696653505793563, 20.00000000000000355 ) ) ;
#5808 = PLANE ( 'NONE',  #6807 ) ;
#5809 = ORIENTED_EDGE ( 'NONE', *, *, #10218, .T. ) ;
#5810 = FACE_OUTER_BOUND ( 'NONE', #203, .T. ) ;
#5811 = CIRCLE ( 'NONE', #4629, 7.500000000000000000 ) ;
#5812 = ORIENTED_EDGE ( 'NONE', *, *, #3524, .T. ) ;
#5813 = DIRECTION ( 'NONE',  ( 1.000000000000000000, 0.000000000000000000, -9.101836848464096770E-17 ) ) ;
#5814 = DIRECTION ( 'NONE',  ( 0.000000000000000000, 0.000000000000000000, 1.000000000000000000 ) ) ;
#5815 = AXIS2_PLACEMENT_3D ( 'NONE', #7565, #9148, #4277 ) ;
#5816 = CARTESIAN_POINT ( 'NONE',  ( 0.000000000000000000, -2.935248768560057009, 4.770489558936219510E-15 ) ) ;
#5817 = DIRECTION ( 'NONE',  ( 0.000000000000000000, 0.000000000000000000, 1.000000000000000000 ) ) ;
#5818 = LINE ( 'NONE', #9055, #9398 ) ;
#5819 = PLANE ( 'NONE',  #261 ) ;
#5820 = ADVANCED_FACE ( 'NONE', ( #4020 ), #7891, .F. ) ;
#5821 = ORIENTED_EDGE ( 'NONE', *, *, #731, .F. ) ;
#5822 = ORIENTED_EDGE ( 'NONE', *, *, #4635, .F. ) ;
#5823 = VERTEX_POINT ( 'NONE', #6845 ) ;
#5824 = DIRECTION ( 'NONE',  ( -0.9936146452197298640, 0.000000000000000000, -0.1128270216077269933 ) ) ;
#5825 = CARTESIAN_POINT ( 'NONE',  ( -43.93820948810023452, 0.000000000000000000, 0.000000000000000000 ) ) ;
#5826 = VECTOR ( 'NONE', #8717, 1000.000000000000114 ) ;
#5827 = CARTESIAN_POINT ( 'NONE',  ( -23.15769640663940976, -117.1457019118819005, 47.99999999999997868 ) ) ;
#5828 = LINE ( 'NONE', #7478, #5540 ) ;
#5829 = AXIS2_PLACEMENT_3D ( 'NONE', #7362, #2536, #8264 ) ;
#5830 = PLANE ( 'NONE',  #3335 ) ;
#5831 = ORIENTED_EDGE ( 'NONE', *, *, #6125, .T. ) ;
#5832 = CARTESIAN_POINT ( 'NONE',  ( -117.0000000000000000, -0.2735269159956698060, 3.990636919869545718 ) ) ;
#5833 = EDGE_CURVE ( 'NONE', #4585, #249, #5628, .T. ) ;
#5834 = CIRCLE ( 'NONE', #6520, 4.000000000000000000 ) ;
#5835 = EDGE_LOOP ( 'NONE', ( #4032, #6728, #5967, #440 ) ) ;
#5836 = ORIENTED_EDGE ( 'NONE', *, *, #1336, .T. ) ;
#5837 = DIRECTION ( 'NONE',  ( 0.000000000000000000, -1.000000000000000000, 0.000000000000000000 ) ) ;
#5838 = LINE ( 'NONE', #1072, #7303 ) ;
#5839 = CARTESIAN_POINT ( 'NONE',  ( 3.000000000000000000, -3.380207847158608363E-15, -2.541999999999999815 ) ) ;
#5840 = CARTESIAN_POINT ( 'NONE',  ( -106.6701082104768687, 217.3094976449379203, 0.000000000000000000 ) ) ;
#5841 = FACE_OUTER_BOUND ( 'NONE', #525, .T. ) ;
#5842 = CARTESIAN_POINT ( 'NONE',  ( 37.51004848672140923, -135.0890599259516875, -26.66894625761717563 ) ) ;
#5843 = AXIS2_PLACEMENT_3D ( 'NONE', #5907, #8350, #458 ) ;
#5844 = ORIENTED_EDGE ( 'NONE', *, *, #7806, .F. ) ;
#5845 = DIRECTION ( 'NONE',  ( 0.000000000000000000, -0.000000000000000000, 1.000000000000000000 ) ) ;
#5846 = EDGE_CURVE ( 'NONE', #4758, #3180, #893, .T. ) ;
#5847 = EDGE_CURVE ( 'NONE', #7273, #3785, #10386, .T. ) ;
#5848 = ORIENTED_EDGE ( 'NONE', *, *, #10252, .T. ) ;
#5849 = VECTOR ( 'NONE', #5101, 1000.000000000000000 ) ;
#5850 = DIRECTION ( 'NONE',  ( 0.000000000000000000, 0.5735764363510476027, -0.8191520442889906883 ) ) ;
#5851 = EDGE_LOOP ( 'NONE', ( #3853, #8103 ) ) ;
#5852 = AXIS2_PLACEMENT_3D ( 'NONE', #1822, #5255, #9241 ) ;
#5853 = LINE ( 'NONE', #6009, #1977 ) ;
#5854 = DIRECTION ( 'NONE',  ( -0.000000000000000000, 1.000000000000000000, -0.000000000000000000 ) ) ;
#5855 = LINE ( 'NONE', #2524, #5675 ) ;
#5856 = AXIS2_PLACEMENT_3D ( 'NONE', #10250, #1183, #2189 ) ;
#5857 = EDGE_CURVE ( 'NONE', #4869, #2362, #5295, .T. ) ;
#5858 = EDGE_CURVE ( 'NONE', #5268, #1613, #6731, .T. ) ;
#5859 = EDGE_CURVE ( 'NONE', #9506, #3747, #7103, .T. ) ;
#5860 = ORIENTED_EDGE ( 'NONE', *, *, #1427, .F. ) ;
#5861 = DIRECTION ( 'NONE',  ( -1.000000000000000000, -0.000000000000000000, -0.000000000000000000 ) ) ;
#5862 = VECTOR ( 'NONE', #782, 1000.000000000000000 ) ;
#5863 = VERTEX_POINT ( 'NONE', #6293 ) ;
#5864 = LINE ( 'NONE', #3276, #816 ) ;
#5865 = LINE ( 'NONE', #4027, #6113 ) ;
#5866 = DIRECTION ( 'NONE',  ( 0.000000000000000000, -1.000000000000000000, 0.000000000000000000 ) ) ;
#5867 = CIRCLE ( 'NONE', #3846, 4.000000000000000000 ) ;
#5868 = CARTESIAN_POINT ( 'NONE',  ( -30.29350689640809335, -0.3998014571812398832, -1.076388538564875708 ) ) ;
#5869 = DIRECTION ( 'NONE',  ( -1.000000000000000000, 0.000000000000000000, 0.000000000000000000 ) ) ;
#5870 = CARTESIAN_POINT ( 'NONE',  ( -50.00000000000002132, -133.1457019118818721, 23.15769640663938134 ) ) ;
#5871 = VECTOR ( 'NONE', #9991, 1000.000000000000000 ) ;
#5872 = EDGE_CURVE ( 'NONE', #2948, #6283, #1152, .T. ) ;
#5873 = ORIENTED_EDGE ( 'NONE', *, *, #2808, .F. ) ;
#5874 = ORIENTED_EDGE ( 'NONE', *, *, #5738, .T. ) ;
#5875 = AXIS2_PLACEMENT_3D ( 'NONE', #5297, #8537, #4510 ) ;
#5876 = ORIENTED_EDGE ( 'NONE', *, *, #3686, .F. ) ;
#5877 = ORIENTED_EDGE ( 'NONE', *, *, #4240, .T. ) ;
#5878 = ADVANCED_FACE ( 'NONE', ( #3271 ), #8942, .F. ) ;
#5879 = DIRECTION ( 'NONE',  ( 0.000000000000000000, 0.000000000000000000, 1.000000000000000000 ) ) ;
#5880 = EDGE_CURVE ( 'NONE', #8070, #2974, #44, .T. ) ;
#5881 = DIRECTION ( 'NONE',  ( 0.000000000000000000, 1.000000000000000000, 1.460512169908342690E-16 ) ) ;
#5882 = VECTOR ( 'NONE', #6678, 1000.000000000000000 ) ;
#5883 = CARTESIAN_POINT ( 'NONE',  ( 3.000000000000000000, 1.467624384280025174, -2.542000000000001592 ) ) ;
#5884 = LINE ( 'NONE', #224, #10122 ) ;
#5885 = ORIENTED_EDGE ( 'NONE', *, *, #5006, .T. ) ;
#5886 = FACE_OUTER_BOUND ( 'NONE', #412, .T. ) ;
#5887 = ORIENTED_EDGE ( 'NONE', *, *, #9037, .F. ) ;
#5888 = CARTESIAN_POINT ( 'NONE',  ( -47.94539818030328604, 155.5289575273811522, 0.000000000000000000 ) ) ;
#5889 = CIRCLE ( 'NONE', #8091, 3.999999999999996447 ) ;
#5890 = ORIENTED_EDGE ( 'NONE', *, *, #9890, .T. ) ;
#5891 = PRODUCT_DEFINITION_CONTEXT ( 'detailed design', #10047, 'design' ) ;
#5892 = DIRECTION ( 'NONE',  ( 0.000000000000000000, -1.000000000000000000, 0.000000000000000000 ) ) ;
#5893 = CARTESIAN_POINT ( 'NONE',  ( 39.99999999999997158, -145.1457019118819005, 35.99999999999999289 ) ) ;
#5894 = DIRECTION ( 'NONE',  ( 0.000000000000000000, -1.000000000000000000, -1.222897680782651471E-16 ) ) ;
#5895 = DIRECTION ( 'NONE',  ( 0.000000000000000000, 0.000000000000000000, 1.000000000000000000 ) ) ;
#5896 = CIRCLE ( 'NONE', #10474, 5.000000000000004441 ) ;
#5897 = CARTESIAN_POINT ( 'NONE',  ( 37.22759939293836595, -133.2806705862436729, -25.15769640663938489 ) ) ;
#5898 = ORIENTED_EDGE ( 'NONE', *, *, #9521, .T. ) ;
#5899 = CIRCLE ( 'NONE', #4552, 4.700000000000000178 ) ;
#5900 = CARTESIAN_POINT ( 'NONE',  ( -39.65557114539781480, 3.552635616211504477, -1.840410121656756326 ) ) ;
#5901 = ORIENTED_EDGE ( 'NONE', *, *, #1440, .T. ) ;
#5902 = LINE ( 'NONE', #2675, #8444 ) ;
#5903 = ORIENTED_EDGE ( 'NONE', *, *, #934, .F. ) ;
#5904 = VECTOR ( 'NONE', #210, 1000.000000000000000 ) ;
#5905 = EDGE_CURVE ( 'NONE', #2739, #10107, #5287, .T. ) ;
#5906 = FACE_OUTER_BOUND ( 'NONE', #1640, .T. ) ;
#5907 = CARTESIAN_POINT ( 'NONE',  ( 14.70649310359190309, 80.56966535057935630, 20.00000000000000711 ) ) ;
#5908 = CARTESIAN_POINT ( 'NONE',  ( -16.29350689640809691, -7.660287962196459688, -7.499999999999998224 ) ) ;
#5909 = EDGE_CURVE ( 'NONE', #4261, #954, #2580, .T. ) ;
#5910 = CARTESIAN_POINT ( 'NONE',  ( -43.93820948810023452, 4.898587196589412829E-16, -4.000000000000000000 ) ) ;
#5911 = VECTOR ( 'NONE', #8572, 1000.000000000000000 ) ;
#5912 = VERTEX_POINT ( 'NONE', #3480 ) ;
#5913 = FACE_OUTER_BOUND ( 'NONE', #2590, .T. ) ;
#5914 = ORIENTED_EDGE ( 'NONE', *, *, #6583, .F. ) ;
#5915 = DIRECTION ( 'NONE',  ( -1.000000000000000000, -0.000000000000000000, -0.000000000000000000 ) ) ;
#5916 = EDGE_CURVE ( 'NONE', #826, #7105, #4674, .T. ) ;
#5917 = CARTESIAN_POINT ( 'NONE',  ( -20.29350689640809691, 140.5696653505793563, 20.00000000000002132 ) ) ;
#5918 = ADVANCED_FACE ( 'NONE', ( #8139 ), #7405, .F. ) ;
#5919 = EDGE_CURVE ( 'NONE', #5357, #5066, #220, .T. ) ;
#5920 = DIRECTION ( 'NONE',  ( 0.07334937666141724821, -0.9973063064792989652, 0.000000000000000000 ) ) ;
#5921 = DIRECTION ( 'NONE',  ( -0.000000000000000000, 1.000000000000000000, -0.000000000000000000 ) ) ;
#5922 = CARTESIAN_POINT ( 'NONE',  ( 6.756858349438879863, 146.7073643690755773, -30.00000000000000355 ) ) ;
#5923 = CARTESIAN_POINT ( 'NONE',  ( -30.29350689640809335, 112.5696653505793705, -20.00000000000000711 ) ) ;
#5924 = ORIENTED_EDGE ( 'NONE', *, *, #5335, .F. ) ;
#5925 = VERTEX_POINT ( 'NONE', #9962 ) ;
#5926 = VERTEX_POINT ( 'NONE', #9910 ) ;
#5927 = DIRECTION ( 'NONE',  ( 0.000000000000000000, 0.000000000000000000, 1.000000000000000000 ) ) ;
#5928 = DIRECTION ( 'NONE',  ( 1.000000000000000000, 0.000000000000000000, 0.000000000000000000 ) ) ;
#5929 = ADVANCED_FACE ( 'NONE', ( #1732 ), #1680, .T. ) ;
#5930 = DIRECTION ( 'NONE',  ( -0.000000000000000000, -0.000000000000000000, -1.000000000000000000 ) ) ;
#5931 = CARTESIAN_POINT ( 'NONE',  ( -21.29350689640810046, 105.5289575273812233, -7.749999999999995559 ) ) ;
#5932 = CIRCLE ( 'NONE', #3398, 4.295524112943372330 ) ;
#5933 = VERTEX_POINT ( 'NONE', #9100 ) ;
#5934 = DIRECTION ( 'NONE',  ( -1.000000000000000000, 0.000000000000000000, 0.000000000000000000 ) ) ;
#5935 = ORIENTED_EDGE ( 'NONE', *, *, #2172, .T. ) ;
#5936 = FILL_AREA_STYLE ('',( #10084 ) ) ;
#5937 = AXIS2_PLACEMENT_3D ( 'NONE', #5159, #9949, #1135 ) ;
#5938 = EDGE_LOOP ( 'NONE', ( #1925, #6340 ) ) ;
#5939 = VECTOR ( 'NONE', #9075, 1000.000000000000000 ) ;
#5940 = DIRECTION ( 'NONE',  ( 0.000000000000000000, -1.000000000000000000, -0.000000000000000000 ) ) ;
#5941 = CYLINDRICAL_SURFACE ( 'NONE', #3661, 10.00000000000000178 ) ;
#5942 = FACE_OUTER_BOUND ( 'NONE', #4421, .T. ) ;
#5943 = FACE_OUTER_BOUND ( 'NONE', #5486, .T. ) ;
#5944 = CARTESIAN_POINT ( 'NONE',  ( -27.85255513972543895, 90.52895752738122326, 7.750000000000002665 ) ) ;
#5945 = AXIS2_PLACEMENT_3D ( 'NONE', #7359, #9053, #6668 ) ;
#5946 = VERTEX_POINT ( 'NONE', #4120 ) ;
#5947 = TOROIDAL_SURFACE ( 'NONE', #9523, 4.000000000000000000, 2.000000000000000000 ) ;
#5948 = CARTESIAN_POINT ( 'NONE',  ( -39.65624476065124782, -3.117691453623975484, -1.800000000000017586 ) ) ;
#5949 = ADVANCED_FACE ( 'NONE', ( #1784 ), #5808, .T. ) ;
#5950 = ORIENTED_EDGE ( 'NONE', *, *, #4425, .F. ) ;
#5951 = PLANE ( 'NONE',  #5229 ) ;
#5952 = ORIENTED_EDGE ( 'NONE', *, *, #5599, .T. ) ;
#5953 = TOROIDAL_SURFACE ( 'NONE', #10032, 16.62298474266377468, 9.050254677131421843 ) ;
#5954 = AXIS2_PLACEMENT_3D ( 'NONE', #6661, #2471, #5698 ) ;
#5955 =( LENGTH_UNIT ( ) NAMED_UNIT ( * ) SI_UNIT ( .MILLI., .METRE. ) );
#5956 = FACE_OUTER_BOUND ( 'NONE', #1364, .T. ) ;
#5957 = FACE_OUTER_BOUND ( 'NONE', #3555, .T. ) ;
#5958 = DIRECTION ( 'NONE',  ( 0.000000000000000000, 0.000000000000000000, 1.000000000000000000 ) ) ;
#5959 = DIRECTION ( 'NONE',  ( 0.000000000000000000, 0.000000000000000000, -1.000000000000000000 ) ) ;
#5960 = ORIENTED_EDGE ( 'NONE', *, *, #1707, .T. ) ;
#5961 = DIRECTION ( 'NONE',  ( 0.000000000000000000, 0.000000000000000000, 1.000000000000000000 ) ) ;
#5962 = VECTOR ( 'NONE', #1599, 1000.000000000000000 ) ;
#5963 = CIRCLE ( 'NONE', #3775, 1.999999999999998224 ) ;
#5964 = ORIENTED_EDGE ( 'NONE', *, *, #5096, .T. ) ;
#5965 = DIRECTION ( 'NONE',  ( 0.9327526414309301739, -0.3605170036262129729, 0.000000000000000000 ) ) ;
#5966 = EDGE_CURVE ( 'NONE', #8839, #6132, #1836, .T. ) ;
#5967 = ORIENTED_EDGE ( 'NONE', *, *, #9521, .F. ) ;
#5968 = CARTESIAN_POINT ( 'NONE',  ( -148.7787556848684858, 265.7124323042283436, 9.545148955221437884E-16 ) ) ;
#5969 = ORIENTED_EDGE ( 'NONE', *, *, #7672, .T. ) ;
#5970 = DIRECTION ( 'NONE',  ( 1.396588258780021135E-16, -0.000000000000000000, 1.000000000000000000 ) ) ;
#5971 = CARTESIAN_POINT ( 'NONE',  ( -7.293506896408105789, 128.5696653505793563, -20.00000000000000711 ) ) ;
#5972 = CARTESIAN_POINT ( 'NONE',  ( -8.000000000000000000, 0.000000000000000000, 0.000000000000000000 ) ) ;
#5973 = DIRECTION ( 'NONE',  ( 0.000000000000000000, 0.000000000000000000, -1.000000000000000000 ) ) ;
#5974 = CARTESIAN_POINT ( 'NONE',  ( -16.29350689640809691, 37.08684478514406635, 0.000000000000000000 ) ) ;
#5975 = FACE_OUTER_BOUND ( 'NONE', #170, .T. ) ;
#5976 = ORIENTED_EDGE ( 'NONE', *, *, #7327, .T. ) ;
#5977 = EDGE_CURVE ( 'NONE', #2542, #1967, #3379, .T. ) ;
#5978 = ORIENTED_EDGE ( 'NONE', *, *, #6039, .F. ) ;
#5979 = VECTOR ( 'NONE', #8208, 1000.000000000000000 ) ;
#5980 = EDGE_CURVE ( 'NONE', #6514, #7036, #722, .T. ) ;
#5981 = CIRCLE ( 'NONE', #10413, 2.515249034521771510 ) ;
#5982 = DIRECTION ( 'NONE',  ( -0.000000000000000000, -1.000000000000000000, -0.000000000000000000 ) ) ;
#5983 = DIRECTION ( 'NONE',  ( 0.000000000000000000, 0.000000000000000000, 1.000000000000000000 ) ) ;
#5984 = PLANE ( 'NONE',  #6652 ) ;
#5985 = CARTESIAN_POINT ( 'NONE',  ( -3.173844575093148990, 90.52895752738122326, 7.750000000000000000 ) ) ;
#5986 = AXIS2_PLACEMENT_3D ( 'NONE', #6394, #4704, #10379 ) ;
#5987 = EDGE_LOOP ( 'NONE', ( #6477, #466, #8745, #9718 ) ) ;
#5988 = CARTESIAN_POINT ( 'NONE',  ( 53.40242741783141156, 147.5696653505793279, -30.00000000000000355 ) ) ;
#5989 = PRODUCT_DEFINITION_FORMATION_WITH_SPECIFIED_SOURCE ( 'ANY', '', #8052, .NOT_KNOWN. ) ;
#5990 = ORIENTED_EDGE ( 'NONE', *, *, #10239, .F. ) ;
#5991 = DIRECTION ( 'NONE',  ( -0.000000000000000000, 1.000000000000000000, -0.000000000000000000 ) ) ;
#5992 = ADVANCED_FACE ( 'NONE', ( #989 ), #6607, .T. ) ;
#5993 = EDGE_CURVE ( 'NONE', #477, #5926, #7487, .T. ) ;
#5994 = VERTEX_POINT ( 'NONE', #5910 ) ;
#5995 = DIRECTION ( 'NONE',  ( 1.000000000000000000, 0.000000000000000000, 8.379529552680125332E-16 ) ) ;
#5996 = CARTESIAN_POINT ( 'NONE',  ( -7.293506896408097795, 4.007378841484243628E-15, -28.00000000000002132 ) ) ;
#5997 = DIRECTION ( 'NONE',  ( -0.7431448254773957984, 0.6691306063588565722, -0.000000000000000000 ) ) ;
#5998 = DIRECTION ( 'NONE',  ( 0.000000000000000000, 0.000000000000000000, 1.000000000000000000 ) ) ;
#5999 = FACE_OUTER_BOUND ( 'NONE', #3778, .T. ) ;
#6000 = TOROIDAL_SURFACE ( 'NONE', #1096, 11.15107097094592881, 2.515249034521771510 ) ;
#6001 = VERTEX_POINT ( 'NONE', #257 ) ;
#6002 = CARTESIAN_POINT ( 'NONE',  ( -56.36957570605427037, 137.0132282531173473, 0.000000000000000000 ) ) ;
#6003 = CIRCLE ( 'NONE', #2624, 3.999999999999976019 ) ;
#6004 = EDGE_LOOP ( 'NONE', ( #9790, #10451, #6425, #5098 ) ) ;
#6005 = DIRECTION ( 'NONE',  ( 1.000000000000000000, -0.000000000000000000, -0.000000000000000000 ) ) ;
#6006 = CARTESIAN_POINT ( 'NONE',  ( -2.293506896408094242, 152.5696653505793279, 12.50000000000000000 ) ) ;
#6007 = EDGE_CURVE ( 'NONE', #7514, #9202, #6712, .T. ) ;
#6008 = VECTOR ( 'NONE', #6188, 1000.000000000000000 ) ;
#6009 = CARTESIAN_POINT ( 'NONE',  ( -47.94539818030330025, 150.5696653505793563, 3.999999999999993339 ) ) ;
#6010 = DIRECTION ( 'NONE',  ( -0.6761648913424331830, 0.7367503238654705688, 0.000000000000000000 ) ) ;
#6011 = CYLINDRICAL_SURFACE ( 'NONE', #609, 3.999999999999989786 ) ;
#6012 = LINE ( 'NONE', #4429, #2231 ) ;
#6013 = ORIENTED_EDGE ( 'NONE', *, *, #871, .F. ) ;
#6014 = CARTESIAN_POINT ( 'NONE',  ( -23.79350689640809691, 120.5289575273812233, 7.750000000000007105 ) ) ;
#6015 = AXIS2_PLACEMENT_3D ( 'NONE', #3546, #6770, #367 ) ;
#6016 = ORIENTED_EDGE ( 'NONE', *, *, #8566, .T. ) ;
#6017 = ORIENTED_EDGE ( 'NONE', *, *, #4516, .F. ) ;
#6018 = AXIS2_PLACEMENT_3D ( 'NONE', #3954, #6333, #7184 ) ;
#6019 = DIRECTION ( 'NONE',  ( 0.000000000000000000, 0.000000000000000000, 1.000000000000000000 ) ) ;
#6020 = ORIENTED_EDGE ( 'NONE', *, *, #6202, .F. ) ;
#6021 = DIRECTION ( 'NONE',  ( -0.6691306063588564612, -0.7431448254773957984, 0.000000000000000000 ) ) ;
#6022 = DIRECTION ( 'NONE',  ( 0.000000000000000000, 0.000000000000000000, 1.000000000000000000 ) ) ;
#6023 = CIRCLE ( 'NONE', #9774, 7.999999999999996447 ) ;
#6024 = CARTESIAN_POINT ( 'NONE',  ( 3.000000000000000000, 1.467624384280025174, -2.542000000000001592 ) ) ;
#6025 = CARTESIAN_POINT ( 'NONE',  ( -27.15769640663939555, -117.1457019118819005, -23.15769640663944173 ) ) ;
#6026 = ADVANCED_FACE ( 'NONE', ( #10213 ), #511, .T. ) ;
#6027 = DIRECTION ( 'NONE',  ( -0.9973063064792990762, -0.07334937666141773394, 0.000000000000000000 ) ) ;
#6028 = FACE_OUTER_BOUND ( 'NONE', #3705, .T. ) ;
#6029 = ORIENTED_EDGE ( 'NONE', *, *, #2414, .T. ) ;
#6030 = VERTEX_POINT ( 'NONE', #9361 ) ;
#6031 = VECTOR ( 'NONE', #3119, 1000.000000000000000 ) ;
#6032 = DIRECTION ( 'NONE',  ( -0.000000000000000000, -0.000000000000000000, -1.000000000000000000 ) ) ;
#6033 = AXIS2_PLACEMENT_3D ( 'NONE', #10459, #8223, #7326 ) ;
#6034 = AXIS2_PLACEMENT_3D ( 'NONE', #2086, #3045, #4579 ) ;
#6035 = ORIENTED_EDGE ( 'NONE', *, *, #6379, .F. ) ;
#6036 = DIRECTION ( 'NONE',  ( 0.000000000000000000, 0.000000000000000000, -1.000000000000000000 ) ) ;
#6037 = CARTESIAN_POINT ( 'NONE',  ( 37.22759939293836595, -116.8755810935459181, -25.15769640663939910 ) ) ;
#6038 = DIRECTION ( 'NONE',  ( -0.6691306063588549069, -0.7431448254773971307, 0.000000000000000000 ) ) ;
#6039 = EDGE_CURVE ( 'NONE', #6250, #8639, #2582, .T. ) ;
#6040 = CARTESIAN_POINT ( 'NONE',  ( 23.76520584195949226, -145.1457019118819005, 49.99999999999997868 ) ) ;
#6041 = CIRCLE ( 'NONE', #1483, 4.729641367753004033 ) ;
#6042 = ORIENTED_EDGE ( 'NONE', *, *, #5557, .F. ) ;
#6043 = VERTEX_POINT ( 'NONE', #10108 ) ;
#6044 = AXIS2_PLACEMENT_3D ( 'NONE', #10240, #9387, #2806 ) ;
#6045 = DIRECTION ( 'NONE',  ( 9.776117811460147207E-16, -0.000000000000000000, -1.000000000000000000 ) ) ;
#6046 = AXIS2_PLACEMENT_3D ( 'NONE', #2129, #2870, #8438 ) ;
#6047 = ORIENTED_EDGE ( 'NONE', *, *, #7593, .T. ) ;
#6048 = ORIENTED_EDGE ( 'NONE', *, *, #1542, .F. ) ;
#6049 = CARTESIAN_POINT ( 'NONE',  ( -2.293506896408097795, 152.5696653505793279, 12.50000000000000000 ) ) ;
#6050 = CARTESIAN_POINT ( 'NONE',  ( -55.94539818030328604, 145.0132282531173189, 3.999999999999990230 ) ) ;
#6051 = DIRECTION ( 'NONE',  ( -1.000000000000000000, -0.000000000000000000, -0.000000000000000000 ) ) ;
#6052 = DIRECTION ( 'NONE',  ( 0.6585271261848795188, -0.7525569905852207420, -2.609853011491003364E-16 ) ) ;
#6053 = EDGE_CURVE ( 'NONE', #7959, #8633, #9203, .T. ) ;
#6054 = EDGE_CURVE ( 'NONE', #1695, #4328, #4449, .T. ) ;
#6055 = ADVANCED_FACE ( 'NONE', ( #6121 ), #2838, .F. ) ;
#6056 = CARTESIAN_POINT ( 'NONE',  ( -16.29350689640809691, 88.12362273389504708, 0.000000000000000000 ) ) ;
#6057 = AXIS2_PLACEMENT_3D ( 'NONE', #4403, #7632, #6036 ) ;
#6058 = ORIENTED_EDGE ( 'NONE', *, *, #6932, .T. ) ;
#6059 = LINE ( 'NONE', #8342, #1906 ) ;
#6060 = CIRCLE ( 'NONE', #1501, 10.00000000000000178 ) ;
#6061 = CARTESIAN_POINT ( 'NONE',  ( -7.293506896408097795, 2.445795361565304815E-15, -20.00000000000002132 ) ) ;
#6062 = VECTOR ( 'NONE', #432, 1000.000000000000000 ) ;
#6063 = EDGE_CURVE ( 'NONE', #9794, #4419, #5456, .T. ) ;
#6064 = LINE ( 'NONE', #8403, #6547 ) ;
#6065 = COLOUR_RGB ( '',0.7921568627450980005, 0.8196078431372548767, 0.9333333333333333481 ) ;
#6066 = CARTESIAN_POINT ( 'NONE',  ( 37.65642917125824596, -135.1457019118819005, 27.03600932663011847 ) ) ;
#6067 = SPHERICAL_SURFACE ( 'NONE', #3654, 8.000000000000000000 ) ;
#6068 = DIRECTION ( 'NONE',  ( -1.000000000000000000, 0.000000000000000000, 0.000000000000000000 ) ) ;
#6069 = ORIENTED_EDGE ( 'NONE', *, *, #7322, .T. ) ;
#6070 = DIRECTION ( 'NONE',  ( -1.000000000000000000, 0.000000000000000000, -0.000000000000000000 ) ) ;
#6071 = CARTESIAN_POINT ( 'NONE',  ( 0.000000000000000000, 0.000000000000000000, 0.000000000000000000 ) ) ;
#6072 = VERTEX_POINT ( 'NONE', #7715 ) ;
#6073 = DIRECTION ( 'NONE',  ( 0.6585271261848804070, -0.7525569905852197428, -0.000000000000000000 ) ) ;
#6074 = AXIS2_PLACEMENT_3D ( 'NONE', #4302, #8147, #9107 ) ;
#6075 = VERTEX_POINT ( 'NONE', #6014 ) ;
#6076 = ORIENTED_EDGE ( 'NONE', *, *, #8687, .F. ) ;
#6077 = LINE ( 'NONE', #2898, #5562 ) ;
#6078 = PLANE ( 'NONE',  #6806 ) ;
#6079 = VERTEX_POINT ( 'NONE', #8561 ) ;
#6080 = CARTESIAN_POINT ( 'NONE',  ( -40.00000000000002842, -145.1457019118819005, 39.99999999999997868 ) ) ;
#6081 = CARTESIAN_POINT ( 'NONE',  ( -48.00000000000002132, -133.1457019118818721, 23.15769640663938134 ) ) ;
#6082 = DIRECTION ( 'NONE',  ( 1.000000000000000000, 0.000000000000000000, 0.000000000000000000 ) ) ;
#6083 = CARTESIAN_POINT ( 'NONE',  ( -36.36957570605426326, 137.0132282531173473, 4.000000000000003553 ) ) ;
#6084 = VECTOR ( 'NONE', #8484, 1000.000000000000000 ) ;
#6085 = VERTEX_POINT ( 'NONE', #3743 ) ;
#6086 = EDGE_CURVE ( 'NONE', #6250, #6120, #2890, .T. ) ;
#6087 = VERTEX_POINT ( 'NONE', #9313 ) ;
#6088 = CARTESIAN_POINT ( 'NONE',  ( 4.856471286862175774, 152.5696653505793279, 25.00000000000000000 ) ) ;
#6089 = ORIENTED_EDGE ( 'NONE', *, *, #1831, .T. ) ;
#6090 = DIRECTION ( 'NONE',  ( -1.000000000000000000, 0.000000000000000000, 0.000000000000000000 ) ) ;
#6091 = DIRECTION ( 'NONE',  ( 0.000000000000000000, 0.000000000000000000, 1.000000000000000000 ) ) ;
#6092 = DIRECTION ( 'NONE',  ( -0.000000000000000000, 1.000000000000000000, -0.000000000000000000 ) ) ;
#6093 = DIRECTION ( 'NONE',  ( -7.016001027857731783E-17, 0.8191520442889911324, -0.5735764363510471586 ) ) ;
#6094 = VERTEX_POINT ( 'NONE', #8511 ) ;
#6095 = ORIENTED_EDGE ( 'NONE', *, *, #4375, .T. ) ;
#6096 = EDGE_CURVE ( 'NONE', #2136, #847, #8458, .T. ) ;
#6097 = ORIENTED_EDGE ( 'NONE', *, *, #5499, .T. ) ;
#6098 = ORIENTED_EDGE ( 'NONE', *, *, #7309, .F. ) ;
#6099 = CARTESIAN_POINT ( 'NONE',  ( 27.15769640663940621, -135.1457019118818721, -48.00000000000002132 ) ) ;
#6100 = FACE_BOUND ( 'NONE', #1684, .T. ) ;
#6101 = CIRCLE ( 'NONE', #191, 4.729641367753004033 ) ;
#6102 = CARTESIAN_POINT ( 'NONE',  ( -2.293506896408097795, 37.08684478514406635, 30.00000000000000355 ) ) ;
#6103 = DIRECTION ( 'NONE',  ( 0.000000000000000000, 0.000000000000000000, -1.000000000000000000 ) ) ;
#6104 = DIRECTION ( 'NONE',  ( 0.000000000000000000, -1.000000000000000000, 0.000000000000000000 ) ) ;
#6105 = ORIENTED_EDGE ( 'NONE', *, *, #3968, .T. ) ;
#6106 = CARTESIAN_POINT ( 'NONE',  ( -16.29350689640809691, 105.5289575273812233, -10.90000000000000036 ) ) ;
#6107 = VECTOR ( 'NONE', #3086, 1000.000000000000000 ) ;
#6108 = ADVANCED_FACE ( 'NONE', ( #9256 ), #4537, .T. ) ;
#6109 = ADVANCED_FACE ( 'NONE', ( #1887 ), #8332, .T. ) ;
#6110 = ADVANCED_FACE ( 'NONE', ( #5169 ), #8354, .F. ) ;
#6111 = DIRECTION ( 'NONE',  ( -0.6691306063588564612, -0.7431448254773956874, 0.000000000000000000 ) ) ;
#6112 = PLANE ( 'NONE',  #8076 ) ;
#6113 = VECTOR ( 'NONE', #4072, 1000.000000000000114 ) ;
#6114 = CARTESIAN_POINT ( 'NONE',  ( -100.3754516082865393, 204.9375061137627370, 0.000000000000000000 ) ) ;
#6115 = AXIS2_PLACEMENT_3D ( 'NONE', #5825, #4974, #5769 ) ;
#6116 = CARTESIAN_POINT ( 'NONE',  ( -16.29350689640809691, 37.08684478514406635, -7.500000000000000000 ) ) ;
#6117 = DIRECTION ( 'NONE',  ( 0.000000000000000000, 1.000000000000000000, 0.000000000000000000 ) ) ;
#6118 = CARTESIAN_POINT ( 'NONE',  ( -20.29350689640809691, 140.5696653505793563, 10.90000000000000036 ) ) ;
#6119 = EDGE_CURVE ( 'NONE', #7774, #5230, #1094, .T. ) ;
#6120 = VERTEX_POINT ( 'NONE', #6765 ) ;
#6121 = FACE_OUTER_BOUND ( 'NONE', #1566, .T. ) ;
#6122 = ORIENTED_EDGE ( 'NONE', *, *, #5272, .F. ) ;
#6123 = ORIENTED_EDGE ( 'NONE', *, *, #10339, .T. ) ;
#6124 = AXIS2_PLACEMENT_3D ( 'NONE', #919, #2561, #1713 ) ;
#6125 = EDGE_CURVE ( 'NONE', #9884, #4360, #5618, .T. ) ;
#6126 = LINE ( 'NONE', #2098, #1642 ) ;
#6127 = VECTOR ( 'NONE', #938, 1000.000000000000000 ) ;
#6128 = ORIENTED_EDGE ( 'NONE', *, *, #7942, .F. ) ;
#6129 = EDGE_LOOP ( 'NONE', ( #607, #1878, #4959, #597 ) ) ;
#6130 = CARTESIAN_POINT ( 'NONE',  ( -20.14472382240651882, -141.8229441850657793, 28.16739522765904624 ) ) ;
#6131 = DIRECTION ( 'NONE',  ( 0.000000000000000000, -1.000000000000000000, -0.000000000000000000 ) ) ;
#6132 = VERTEX_POINT ( 'NONE', #8408 ) ;
#6133 = CARTESIAN_POINT ( 'NONE',  ( -40.00000000000001421, -135.1457019118818721, -50.00000000000002132 ) ) ;
#6134 = FACE_OUTER_BOUND ( 'NONE', #8318, .T. ) ;
#6135 = DIRECTION ( 'NONE',  ( -0.000000000000000000, -1.000000000000000000, -0.000000000000000000 ) ) ;
#6136 = CIRCLE ( 'NONE', #1567, 2.000000000000001776 ) ;
#6137 = DIRECTION ( 'NONE',  ( -0.9805806756909200006, 0.1698415551216908848, -0.09805806756909091204 ) ) ;
#6138 = AXIS2_PLACEMENT_3D ( 'NONE', #7285, #1720, #867 ) ;
#6139 = ORIENTED_EDGE ( 'NONE', *, *, #6324, .F. ) ;
#6140 = CARTESIAN_POINT ( 'NONE',  ( 0.000000000000000000, -1.467624384280024730, 2.542000000000003368 ) ) ;
#6141 = VECTOR ( 'NONE', #5930, 1000.000000000000000 ) ;
#6142 = ORIENTED_EDGE ( 'NONE', *, *, #4004, .F. ) ;
#6143 = DIRECTION ( 'NONE',  ( -1.000000000000000000, 0.000000000000000000, 0.000000000000000000 ) ) ;
#6144 = DIRECTION ( 'NONE',  ( -1.000000000000000000, 0.000000000000000000, 0.000000000000000000 ) ) ;
#6145 = CYLINDRICAL_SURFACE ( 'NONE', #3615, 4.000000000000000000 ) ;
#6146 = EDGE_CURVE ( 'NONE', #3604, #1079, #9532, .T. ) ;
#6147 = CARTESIAN_POINT ( 'NONE',  ( 42.22511195853867605, 17.84145331825995839, 25.00000000000000000 ) ) ;
#6148 = DIRECTION ( 'NONE',  ( 0.000000000000000000, 0.8660254037844380415, -0.5000000000000012212 ) ) ;
#6149 = ORIENTED_EDGE ( 'NONE', *, *, #7351, .T. ) ;
#6150 = AXIS2_PLACEMENT_3D ( 'NONE', #6025, #9269, #1209 ) ;
#6151 = VERTEX_POINT ( 'NONE', #6385 ) ;
#6152 = ORIENTED_EDGE ( 'NONE', *, *, #7944, .T. ) ;
#6153 = ORIENTED_EDGE ( 'NONE', *, *, #6627, .F. ) ;
#6154 = CARTESIAN_POINT ( 'NONE',  ( 94.78677303995212355, -145.1457019118819005, 30.00000000000000355 ) ) ;
#6155 = FACE_BOUND ( 'NONE', #8431, .T. ) ;
#6156 = AXIS2_PLACEMENT_3D ( 'NONE', #7455, #2633, #3424 ) ;
#6157 = DIRECTION ( 'NONE',  ( 0.000000000000000000, 1.000000000000000000, 0.000000000000000000 ) ) ;
#6158 = CARTESIAN_POINT ( 'NONE',  ( -121.7299640054770578, 230.8694527092982867, 0.000000000000000000 ) ) ;
#6159 = ADVANCED_FACE ( 'NONE', ( #3202 ), #7030, .F. ) ;
#6160 = DIRECTION ( 'NONE',  ( 0.000000000000000000, 0.000000000000000000, -1.000000000000000000 ) ) ;
#6161 = EDGE_LOOP ( 'NONE', ( #2460, #334, #7393, #4931 ) ) ;
#6162 = CYLINDRICAL_SURFACE ( 'NONE', #9161, 5.000000000000004441 ) ;
#6163 = AXIS2_PLACEMENT_3D ( 'NONE', #241, #1821, #2972 ) ;
#6164 = AXIS2_PLACEMENT_3D ( 'NONE', #6883, #5181, #2004 ) ;
#6165 = CARTESIAN_POINT ( 'NONE',  ( 37.71464122736490054, -135.1457019118818721, -27.15769640663940265 ) ) ;
#6166 = AXIS2_PLACEMENT_3D ( 'NONE', #3179, #2379, #4 ) ;
#6167 = LINE ( 'NONE', #5426, #806 ) ;
#6168 = DIRECTION ( 'NONE',  ( 1.000000000000000000, 0.000000000000000000, 1.734723475976805517E-15 ) ) ;
#6169 = EDGE_CURVE ( 'NONE', #7935, #8658, #882, .T. ) ;
#6170 = DIRECTION ( 'NONE',  ( -0.000000000000000000, 1.000000000000000000, -0.000000000000000000 ) ) ;
#6171 = ADVANCED_FACE ( 'NONE', ( #4584 ), #9527, .F. ) ;
#6172 = ORIENTED_EDGE ( 'NONE', *, *, #7289, .F. ) ;
#6173 = DIRECTION ( 'NONE',  ( -0.000000000000000000, 1.000000000000000000, 0.000000000000000000 ) ) ;
#6174 = ORIENTED_EDGE ( 'NONE', *, *, #5258, .F. ) ;
#6175 = PRODUCT_CONTEXT ( 'NONE', #9307, 'mechanical' ) ;
#6176 = ORIENTED_EDGE ( 'NONE', *, *, #6662, .T. ) ;
#6177 = CARTESIAN_POINT ( 'NONE',  ( 10.51964330236497602, 150.0000000000000000, 30.00000000000000355 ) ) ;
#6178 = ORIENTED_EDGE ( 'NONE', *, *, #6096, .T. ) ;
#6179 = AXIS2_PLACEMENT_3D ( 'NONE', #9159, #2053, #3755 ) ;
#6180 = ORIENTED_EDGE ( 'NONE', *, *, #7032, .T. ) ;
#6181 = CARTESIAN_POINT ( 'NONE',  ( -16.29350689640809691, 81.26698356513965393, 4.729641367753003145 ) ) ;
#6182 = FACE_OUTER_BOUND ( 'NONE', #3536, .T. ) ;
#6183 = ORIENTED_EDGE ( 'NONE', *, *, #8765, .T. ) ;
#6184 = DIRECTION ( 'NONE',  ( 0.000000000000000000, 0.000000000000000000, 1.000000000000000000 ) ) ;
#6185 = CARTESIAN_POINT ( 'NONE',  ( 4.856471286862173997, 152.5696653505793279, -12.50000000000000000 ) ) ;
#6186 = EDGE_CURVE ( 'NONE', #4407, #2391, #5431, .T. ) ;
#6187 = ADVANCED_FACE ( 'NONE', ( #3049 ), #3956, .F. ) ;
#6188 = DIRECTION ( 'NONE',  ( -0.000000000000000000, -1.000000000000000000, -0.000000000000000000 ) ) ;
#6189 = ADVANCED_FACE ( 'NONE', ( #8721 ), #7875, .F. ) ;
#6190 = DIRECTION ( 'NONE',  ( -1.000000000000000000, -0.000000000000000000, -0.000000000000000000 ) ) ;
#6191 = DIRECTION ( 'NONE',  ( 0.000000000000000000, 0.000000000000000000, 1.000000000000000000 ) ) ;
#6192 = AXIS2_PLACEMENT_3D ( 'NONE', #8371, #7296, #3214 ) ;
#6193 = ORIENTED_EDGE ( 'NONE', *, *, #1961, .F. ) ;
#6194 = CYLINDRICAL_SURFACE ( 'NONE', #5520, 2.000000000000001776 ) ;
#6195 = EDGE_LOOP ( 'NONE', ( #5326, #7168, #9374, #4616, #784 ) ) ;
#6196 = CARTESIAN_POINT ( 'NONE',  ( -106.6701082104768687, 217.3094976449379203, 0.000000000000000000 ) ) ;
#6197 = FACE_OUTER_BOUND ( 'NONE', #8710, .T. ) ;
#6198 = CONICAL_SURFACE ( 'NONE', #9071, 4.025000000000000355, 0.7853981633975870569 ) ;
#6199 = ORIENTED_EDGE ( 'NONE', *, *, #5543, .F. ) ;
#6200 = CARTESIAN_POINT ( 'NONE',  ( -50.00000000000002132, -134.8487249201535008, 25.28852788137215057 ) ) ;
#6201 = DIRECTION ( 'NONE',  ( 0.000000000000000000, 0.4226182617406934461, 0.9063077870366527122 ) ) ;
#6202 = EDGE_CURVE ( 'NONE', #7686, #5509, #9469, .T. ) ;
#6203 = LINE ( 'NONE', #2179, #5498 ) ;
#6204 = ORIENTED_EDGE ( 'NONE', *, *, #6493, .T. ) ;
#6205 = TOROIDAL_SURFACE ( 'NONE', #6710, 12.02085523418795177, 4.295524112943378547 ) ;
#6206 = VERTEX_POINT ( 'NONE', #7931 ) ;
#6207 = AXIS2_PLACEMENT_3D ( 'NONE', #9433, #3507, #5934 ) ;
#6208 = ADVANCED_FACE ( 'NONE', ( #7187 ), #8616, .F. ) ;
#6209 = ORIENTED_EDGE ( 'NONE', *, *, #142, .T. ) ;
#6210 = ORIENTED_EDGE ( 'NONE', *, *, #8699, .T. ) ;
#6211 = FACE_BOUND ( 'NONE', #7995, .T. ) ;
#6212 = CARTESIAN_POINT ( 'NONE',  ( 25.93998375192765948, -135.0799149511624364, 49.99999999999997868 ) ) ;
#6213 = AXIS2_PLACEMENT_3D ( 'NONE', #9260, #7775, #4435 ) ;
#6214 = LINE ( 'NONE', #1286, #9942 ) ;
#6215 = CARTESIAN_POINT ( 'NONE',  ( -27.15769640663939555, -133.1457019118818721, -27.15769640663944173 ) ) ;
#6216 = AXIS2_PLACEMENT_3D ( 'NONE', #7831, #9646, #10429 ) ;
#6217 = LINE ( 'NONE', #1398, #6884 ) ;
#6218 = ORIENTED_EDGE ( 'NONE', *, *, #5008, .F. ) ;
#6219 = DIRECTION ( 'NONE',  ( -0.7431448254773957984, 0.6691306063588565722, -0.000000000000000000 ) ) ;
#6220 = AXIS2_PLACEMENT_3D ( 'NONE', #183, #132, #6638 ) ;
#6221 = ORIENTED_EDGE ( 'NONE', *, *, #6575, .F. ) ;
#6222 = CIRCLE ( 'NONE', #6044, 4.729641367753004921 ) ;
#6223 = CARTESIAN_POINT ( 'NONE',  ( 49.99999999999997158, -135.1457019118818721, 39.99999999999997868 ) ) ;
#6224 = VECTOR ( 'NONE', #2075, 1000.000000000000114 ) ;
#6225 = DIRECTION ( 'NONE',  ( -0.000000000000000000, 1.000000000000000000, -0.000000000000000000 ) ) ;
#6226 = CARTESIAN_POINT ( 'NONE',  ( -7.293506896408097795, 0.000000000000000000, 0.000000000000000000 ) ) ;
#6227 = ORIENTED_EDGE ( 'NONE', *, *, #6481, .F. ) ;
#6228 = CARTESIAN_POINT ( 'NONE',  ( 27.15769640663936357, -133.1457019118818721, -3.792811993702490094E-15 ) ) ;
#6229 = ORIENTED_EDGE ( 'NONE', *, *, #6850, .T. ) ;
#6230 = APPLICATION_PROTOCOL_DEFINITION ( 'draft international standard', 'automotive_design', 1998, #7680 ) ;
#6231 = VERTEX_POINT ( 'NONE', #614 ) ;
#6232 = CIRCLE ( 'NONE', #8770, 2.000000000000001776 ) ;
#6233 = LINE ( 'NONE', #3746, #1300 ) ;
#6234 = EDGE_CURVE ( 'NONE', #3054, #3508, #6645, .T. ) ;
#6235 = VERTEX_POINT ( 'NONE', #2258 ) ;
#6236 = ORIENTED_EDGE ( 'NONE', *, *, #9064, .T. ) ;
#6237 = DIRECTION ( 'NONE',  ( -1.000000000000000000, 0.000000000000000000, 0.000000000000000000 ) ) ;
#6238 = DIRECTION ( 'NONE',  ( 0.000000000000000000, 0.000000000000000000, -1.000000000000000000 ) ) ;
#6239 = ORIENTED_EDGE ( 'NONE', *, *, #2427, .F. ) ;
#6240 = DIRECTION ( 'NONE',  ( 0.000000000000000000, 0.000000000000000000, 1.000000000000000000 ) ) ;
#6241 = CARTESIAN_POINT ( 'NONE',  ( 3.000000000000000000, 3.113052163432572109E-16, -2.541999999999999815 ) ) ;
#6242 = CARTESIAN_POINT ( 'NONE',  ( 0.000000000000000000, 55.56966535057937051, -10.98204862120179826 ) ) ;
#6243 = DIRECTION ( 'NONE',  ( 0.000000000000000000, 0.000000000000000000, 1.000000000000000000 ) ) ;
#6244 = MECHANICAL_DESIGN_GEOMETRIC_PRESENTATION_REPRESENTATION (  '', ( #1509 ), #1840 ) ;
#6245 = VERTEX_POINT ( 'NONE', #1519 ) ;
#6246 = LINE ( 'NONE', #637, #7727 ) ;
#6247 = ADVANCED_FACE ( 'NONE', ( #3101 ), #551, .F. ) ;
#6248 = EDGE_CURVE ( 'NONE', #1455, #9380, #3249, .T. ) ;
#6249 = EDGE_CURVE ( 'NONE', #869, #7130, #2313, .T. ) ;
#6250 = VERTEX_POINT ( 'NONE', #3153 ) ;
#6251 = CARTESIAN_POINT ( 'NONE',  ( 27.15769640663938489, -115.1457019118818863, -27.15769640663940976 ) ) ;
#6252 = FACE_BOUND ( 'NONE', #9600, .T. ) ;
#6253 =( LENGTH_UNIT ( ) NAMED_UNIT ( * ) SI_UNIT ( .MILLI., .METRE. ) );
#6254 = ORIENTED_EDGE ( 'NONE', *, *, #1904, .T. ) ;
#6255 =( GEOMETRIC_REPRESENTATION_CONTEXT ( 3 ) GLOBAL_UNCERTAINTY_ASSIGNED_CONTEXT ( ( #3950 ) ) GLOBAL_UNIT_ASSIGNED_CONTEXT ( ( #1688, #7307, #53 ) ) REPRESENTATION_CONTEXT ( 'NONE', 'WORKASPACE' ) );
#6256 = DIRECTION ( 'NONE',  ( 1.000000000000000000, 0.000000000000000000, 0.000000000000000000 ) ) ;
#6257 = FACE_OUTER_BOUND ( 'NONE', #7145, .T. ) ;
#6258 = APPLICATION_CONTEXT ( 'automotive_design' ) ;
#6259 = CARTESIAN_POINT ( 'NONE',  ( -16.29350689640809691, -8.635287962196477096, 4.999999999999998224 ) ) ;
#6260 = ORIENTED_EDGE ( 'NONE', *, *, #4501, .T. ) ;
#6261 = VERTEX_POINT ( 'NONE', #717 ) ;
#6262 = EDGE_LOOP ( 'NONE', ( #9221, #4056, #10191, #1205 ) ) ;
#6263 = ADVANCED_FACE ( 'NONE', ( #4006 ), #1401, .F. ) ;
#6264 = ORIENTED_EDGE ( 'NONE', *, *, #9305, .T. ) ;
#6265 = DIRECTION ( 'NONE',  ( -0.6691306063588601249, -0.7431448254773928008, 0.000000000000000000 ) ) ;
#6266 = LINE ( 'NONE', #3395, #3759 ) ;
#6267 = DIRECTION ( 'NONE',  ( -0.000000000000000000, 1.000000000000000000, -0.000000000000000000 ) ) ;
#6268 = CARTESIAN_POINT ( 'NONE',  ( -39.94539818030332157, 145.0132282531173189, 3.999999999999991562 ) ) ;
#6269 = PLANE ( 'NONE',  #7900 ) ;
#6270 = VERTEX_POINT ( 'NONE', #8666 ) ;
#6271 = CARTESIAN_POINT ( 'NONE',  ( 2.275687196221499263E-14, -135.1457019118818721, -27.15769640663943107 ) ) ;
#6272 = ORIENTED_EDGE ( 'NONE', *, *, #8541, .F. ) ;
#6273 = LINE ( 'NONE', #6478, #4527 ) ;
#6274 = CARTESIAN_POINT ( 'NONE',  ( 3.000000000000000000, 1.467624384280033167, 2.541999999999999371 ) ) ;
#6275 = DIRECTION ( 'NONE',  ( -0.000000000000000000, -0.000000000000000000, -1.000000000000000000 ) ) ;
#6276 = EDGE_CURVE ( 'NONE', #4046, #8070, #1382, .T. ) ;
#6277 = DIRECTION ( 'NONE',  ( 0.000000000000000000, 1.000000000000000000, 0.000000000000000000 ) ) ;
#6278 = ORIENTED_EDGE ( 'NONE', *, *, #5513, .F. ) ;
#6279 = AXIS2_PLACEMENT_3D ( 'NONE', #10125, #1951, #3653 ) ;
#6280 = CARTESIAN_POINT ( 'NONE',  ( -40.00000000000001421, -145.1457019118819005, -40.00000000000002132 ) ) ;
#6281 = ORIENTED_EDGE ( 'NONE', *, *, #3140, .F. ) ;
#6282 = DIRECTION ( 'NONE',  ( -0.7431448254773957984, 0.6691306063588565722, -0.000000000000000000 ) ) ;
#6283 = VERTEX_POINT ( 'NONE', #6596 ) ;
#6284 = AXIS2_PLACEMENT_3D ( 'NONE', #6752, #10151, #6859 ) ;
#6285 = CONICAL_SURFACE ( 'NONE', #7642, 4.025000000000000355, 0.7853981633977258348 ) ;
#6286 = ORIENTED_EDGE ( 'NONE', *, *, #5597, .T. ) ;
#6287 = DIRECTION ( 'NONE',  ( -0.6691306063588547959, -0.7431448254773973527, 0.000000000000000000 ) ) ;
#6288 = DIRECTION ( 'NONE',  ( -0.7431448254773957984, 0.6691306063588565722, -0.000000000000000000 ) ) ;
#6289 = CARTESIAN_POINT ( 'NONE',  ( -56.36957570605427748, 150.5696653505793563, -10.90000000000000036 ) ) ;
#6290 = LINE ( 'NONE', #3964, #1429 ) ;
#6291 = DIRECTION ( 'NONE',  ( 0.1124875939035005490, -0.8966615917995903740, 0.4281874951574671795 ) ) ;
#6292 = CARTESIAN_POINT ( 'NONE',  ( 4.856471286862176662, 145.0444252872335937, 25.00000000000000000 ) ) ;
#6293 = CARTESIAN_POINT ( 'NONE',  ( -2.293506896408097795, 145.5696653505793563, 25.00000000000000711 ) ) ;
#6294 = EDGE_CURVE ( 'NONE', #7113, #7523, #977, .T. ) ;
#6295 = CIRCLE ( 'NONE', #3073, 2.000000000000001776 ) ;
#6296 = AXIS2_PLACEMENT_3D ( 'NONE', #849, #2493, #2441 ) ;
#6297 = ORIENTED_EDGE ( 'NONE', *, *, #2280, .F. ) ;
#6298 = CARTESIAN_POINT ( 'NONE',  ( -142.7649729728221359, 249.8094598553370531, 0.000000000000000000 ) ) ;
#6299 = ORIENTED_EDGE ( 'NONE', *, *, #1188, .F. ) ;
#6300 = CARTESIAN_POINT ( 'NONE',  ( -38.96131932220313132, 0.2735269159956709717, 3.990636919869543942 ) ) ;
#6301 = CYLINDRICAL_SURFACE ( 'NONE', #9338, 7.999999999999996447 ) ;
#6302 = AXIS2_PLACEMENT_3D ( 'NONE', #7829, #573, #3808 ) ;
#6303 = ORIENTED_EDGE ( 'NONE', *, *, #8186, .T. ) ;
#6304 = AXIS2_PLACEMENT_3D ( 'NONE', #7563, #1197, #5269 ) ;
#6305 = CARTESIAN_POINT ( 'NONE',  ( 3.000000000000000000, 1.467624384280025174, -2.542000000000001592 ) ) ;
#6306 = DIRECTION ( 'NONE',  ( -1.000000000000000000, -0.000000000000000000, -0.000000000000000000 ) ) ;
#6307 = DIRECTION ( 'NONE',  ( 0.000000000000000000, 0.000000000000000000, -1.000000000000000000 ) ) ;
#6308 = EDGE_LOOP ( 'NONE', ( #1674, #7212, #3256, #10139 ) ) ;
#6309 = EDGE_CURVE ( 'NONE', #3675, #4386, #9682, .T. ) ;
#6310 = EDGE_CURVE ( 'NONE', #6574, #9459, #2622, .T. ) ;
#6311 = EDGE_CURVE ( 'NONE', #6817, #4824, #9705, .T. ) ;
#6312 = ORIENTED_EDGE ( 'NONE', *, *, #1643, .T. ) ;
#6313 = AXIS2_PLACEMENT_3D ( 'NONE', #6215, #3569, #5998 ) ;
#6314 = AXIS2_PLACEMENT_3D ( 'NONE', #3967, #7250, #6349 ) ;
#6315 = ORIENTED_EDGE ( 'NONE', *, *, #6054, .T. ) ;
#6316 = VERTEX_POINT ( 'NONE', #3417 ) ;
#6317 = CARTESIAN_POINT ( 'NONE',  ( 0.000000000000000000, -135.1457019118818721, 0.000000000000000000 ) ) ;
#6318 = DIRECTION ( 'NONE',  ( 0.000000000000000000, -1.000000000000000000, 0.000000000000000000 ) ) ;
#6319 = DIRECTION ( 'NONE',  ( -0.7431448254773957984, 0.6691306063588565722, -0.000000000000000000 ) ) ;
#6320 = CARTESIAN_POINT ( 'NONE',  ( 0.000000000000000000, -145.1457019118819005, 49.99999999999997868 ) ) ;
#6321 = CONICAL_SURFACE ( 'NONE', #2079, 5.025000000000002132, 0.7853981633975176679 ) ;
#6322 = PRODUCT_DEFINITION ( 'UNKNOWN', '', #5989, #182 ) ;
#6323 = DIRECTION ( 'NONE',  ( -0.000000000000000000, 1.000000000000000000, -0.000000000000000000 ) ) ;
#6324 = EDGE_CURVE ( 'NONE', #1005, #9303, #9791, .T. ) ;
#6325 = EDGE_CURVE ( 'NONE', #1057, #1613, #7499, .T. ) ;
#6326 = ORIENTED_EDGE ( 'NONE', *, *, #3849, .F. ) ;
#6327 = FACE_OUTER_BOUND ( 'NONE', #9846, .T. ) ;
#6328 = CIRCLE ( 'NONE', #9717, 3.999999999999989786 ) ;
#6329 = EDGE_LOOP ( 'NONE', ( #5412, #2676, #1662, #6904 ) ) ;
#6330 = DIRECTION ( 'NONE',  ( 0.000000000000000000, -1.000000000000000000, -9.100899318238137994E-17 ) ) ;
#6331 = CARTESIAN_POINT ( 'NONE',  ( -47.94539818030330025, 137.0132282531173473, 3.999999999999991562 ) ) ;
#6332 = CARTESIAN_POINT ( 'NONE',  ( -30.29350689640809335, 37.08684478514406635, 15.00000000000000355 ) ) ;
#6333 = DIRECTION ( 'NONE',  ( 0.000000000000000000, 1.000000000000000000, -1.224646799147353207E-16 ) ) ;
#6334 = AXIS2_PLACEMENT_3D ( 'NONE', #2214, #10227, #1528 ) ;
#6335 = EDGE_LOOP ( 'NONE', ( #9194, #3458, #1965, #4568, #7253, #3901 ) ) ;
#6336 = DIRECTION ( 'NONE',  ( 0.000000000000000000, 0.000000000000000000, -1.000000000000000000 ) ) ;
#6337 = SHAPE_DEFINITION_REPRESENTATION ( #8644, #5747 ) ;
#6338 = ORIENTED_EDGE ( 'NONE', *, *, #3494, .T. ) ;
#6339 = CARTESIAN_POINT ( 'NONE',  ( -1.071796769724492338, 0.000000000000000000, 0.000000000000000000 ) ) ;
#6340 = ORIENTED_EDGE ( 'NONE', *, *, #2869, .F. ) ;
#6341 = EDGE_CURVE ( 'NONE', #7279, #1670, #10208, .T. ) ;
#6342 = AXIS2_PLACEMENT_3D ( 'NONE', #2885, #9358, #10319 ) ;
#6343 = ORIENTED_EDGE ( 'NONE', *, *, #9653, .F. ) ;
#6344 = CARTESIAN_POINT ( 'NONE',  ( -18.34874108452141783, -140.1746510883711778, 24.43989726270226370 ) ) ;
#6345 = LINE ( 'NONE', #3012, #10154 ) ;
#6346 = CARTESIAN_POINT ( 'NONE',  ( -16.29350689640809691, 105.5289575273812233, -25.04213562373096380 ) ) ;
#6347 = CARTESIAN_POINT ( 'NONE',  ( -2.293506896408101348, 150.5696653505793563, 10.98204862120179826 ) ) ;
#6348 = FACE_OUTER_BOUND ( 'NONE', #7524, .T. ) ;
#6349 = DIRECTION ( 'NONE',  ( 1.000000000000000000, 0.000000000000000000, 0.000000000000000000 ) ) ;
#6350 = AXIS2_PLACEMENT_3D ( 'NONE', #1589, #694, #6307 ) ;
#6351 = ORIENTED_EDGE ( 'NONE', *, *, #5786, .T. ) ;
#6352 = DIRECTION ( 'NONE',  ( 0.000000000000000000, 1.000000000000000000, 0.000000000000000000 ) ) ;
#6353 = ORIENTED_EDGE ( 'NONE', *, *, #2945, .F. ) ;
#6354 = CARTESIAN_POINT ( 'NONE',  ( 3.000000000000000000, -2.201436576420041646, 1.271000000000002794 ) ) ;
#6355 = FILL_AREA_STYLE ('',( #7110 ) ) ;
#6356 = VERTEX_POINT ( 'NONE', #7447 ) ;
#6357 = CARTESIAN_POINT ( 'NONE',  ( -30.29350689640809335, 150.5696653505793563, 20.00000000000000711 ) ) ;
#6358 = DIRECTION ( 'NONE',  ( 1.000000000000000000, 0.000000000000000000, 0.000000000000000000 ) ) ;
#6359 = CIRCLE ( 'NONE', #277, 3.999999999999976019 ) ;
#6360 = CYLINDRICAL_SURFACE ( 'NONE', #4314, 3.999999999999989786 ) ;
#6361 = VERTEX_POINT ( 'NONE', #190 ) ;
#6362 = VERTEX_POINT ( 'NONE', #9732 ) ;
#6363 = VECTOR ( 'NONE', #343, 1000.000000000000000 ) ;
#6364 = CIRCLE ( 'NONE', #3839, 3.297986701801175258 ) ;
#6365 = VERTEX_POINT ( 'NONE', #2516 ) ;
#6366 = EDGE_CURVE ( 'NONE', #1028, #9023, #395, .T. ) ;
#6367 = DIRECTION ( 'NONE',  ( -1.000000000000000000, -0.000000000000000000, -0.000000000000000000 ) ) ;
#6368 = LINE ( 'NONE', #8807, #4436 ) ;
#6369 = LINE ( 'NONE', #5518, #10277 ) ;
#6370 = CARTESIAN_POINT ( 'NONE',  ( -50.00000000000002132, -117.1457019118819005, -23.15769640663945594 ) ) ;
#6371 = CARTESIAN_POINT ( 'NONE',  ( -30.29350689640809335, 55.56966535057937051, 10.98204862120179826 ) ) ;
#6372 = AXIS2_PLACEMENT_3D ( 'NONE', #3757, #1963, #335 ) ;
#6373 = VERTEX_POINT ( 'NONE', #8182 ) ;
#6374 = LINE ( 'NONE', #5420, #9686 ) ;
#6375 = AXIS2_PLACEMENT_3D ( 'NONE', #2585, #318, #9103 ) ;
#6376 = ORIENTED_EDGE ( 'NONE', *, *, #3787, .T. ) ;
#6377 = EDGE_CURVE ( 'NONE', #2339, #86, #8238, .T. ) ;
#6378 = DIRECTION ( 'NONE',  ( 1.000000000000000000, 0.000000000000000000, 9.776117811460135374E-16 ) ) ;
#6379 = EDGE_CURVE ( 'NONE', #541, #10221, #6994, .T. ) ;
#6380 = ADVANCED_FACE ( 'NONE', ( #7391 ), #8984, .F. ) ;
#6381 = CARTESIAN_POINT ( 'NONE',  ( 23.40006363390417832, -133.3880685335015812, -50.00000000000001421 ) ) ;
#6382 = LINE ( 'NONE', #7769, #10258 ) ;
#6383 = CIRCLE ( 'NONE', #10116, 2.000000000000001776 ) ;
#6384 = ORIENTED_EDGE ( 'NONE', *, *, #1846, .F. ) ;
#6385 = CARTESIAN_POINT ( 'NONE',  ( -115.9900084698215608, 236.1770707478440841, 9.534008583957946635E-16 ) ) ;
#6386 = VECTOR ( 'NONE', #67, 1000.000000000000000 ) ;
#6387 = APPLICATION_PROTOCOL_DEFINITION ( 'draft international standard', 'automotive_design', 1998, #6791 ) ;
#6388 = ORIENTED_EDGE ( 'NONE', *, *, #1656, .T. ) ;
#6389 = CARTESIAN_POINT ( 'NONE',  ( -23.15769640663937423, -117.1457019118819005, -48.00000000000002132 ) ) ;
#6390 = VERTEX_POINT ( 'NONE', #1771 ) ;
#6391 = VECTOR ( 'NONE', #2384, 1000.000000000000000 ) ;
#6392 = ADVANCED_FACE ( 'NONE', ( #8128 ), #5053, .F. ) ;
#6393 = ORIENTED_EDGE ( 'NONE', *, *, #933, .T. ) ;
#6394 = CARTESIAN_POINT ( 'NONE',  ( -20.29350689640809691, 140.5696653505793563, 0.000000000000000000 ) ) ;
#6395 = FACE_OUTER_BOUND ( 'NONE', #10276, .T. ) ;
#6396 = LINE ( 'NONE', #3061, #4583 ) ;
#6397 = DIRECTION ( 'NONE',  ( 0.000000000000000000, -0.9961946980917445460, -0.08715574274766943463 ) ) ;
#6398 = CIRCLE ( 'NONE', #4033, 3.297986701801175258 ) ;
#6399 = EDGE_LOOP ( 'NONE', ( #843, #5673, #4402, #9258, #3643 ) ) ;
#6400 = CARTESIAN_POINT ( 'NONE',  ( -133.6038276124207300, 241.5607275224312787, 0.000000000000000000 ) ) ;
#6401 = CIRCLE ( 'NONE', #8268, 3.297986701801175258 ) ;
#6402 = ORIENTED_EDGE ( 'NONE', *, *, #615, .T. ) ;
#6403 = CARTESIAN_POINT ( 'NONE',  ( -23.17384457509314899, 130.5696653505793847, 7.750000000000001776 ) ) ;
#6404 = SURFACE_SIDE_STYLE ('',( #1539 ) ) ;
#6405 = TOROIDAL_SURFACE ( 'NONE', #7764, -16.75790667520975674, 26.17065043502059041 ) ;
#6406 = DIRECTION ( 'NONE',  ( -0.000000000000000000, -1.000000000000000000, -0.000000000000000000 ) ) ;
#6407 = DIRECTION ( 'NONE',  ( 0.000000000000000000, 0.000000000000000000, 1.000000000000000000 ) ) ;
#6408 = CARTESIAN_POINT ( 'NONE',  ( -23.15769640663940976, -117.1457019118819005, -1.617088345095243827E-14 ) ) ;
#6409 = VECTOR ( 'NONE', #5260, 1000.000000000000000 ) ;
#6410 = ORIENTED_EDGE ( 'NONE', *, *, #5332, .F. ) ;
#6411 = ADVANCED_FACE ( 'NONE', ( #1029 ), #6485, .T. ) ;
#6412 = EDGE_LOOP ( 'NONE', ( #8400, #178, #6906, #6684, #813, #1602, #6476, #7897, #8568, #8213, #8609, #8327, #7367, #5848 ) ) ;
#6413 = ORIENTED_EDGE ( 'NONE', *, *, #7577, .F. ) ;
#6414 = VECTOR ( 'NONE', #10171, 1000.000000000000114 ) ;
#6415 = FACE_OUTER_BOUND ( 'NONE', #1747, .T. ) ;
#6416 = DIRECTION ( 'NONE',  ( 0.000000000000000000, 1.000000000000000000, 0.000000000000000000 ) ) ;
#6417 = DIRECTION ( 'NONE',  ( 3.081165567444019513E-16, -1.000000000000000000, 0.000000000000000000 ) ) ;
#6418 = DIRECTION ( 'NONE',  ( -6.485608039485835891E-17, -0.9063077870366466060, -0.4226182617407067132 ) ) ;
#6419 = DIRECTION ( 'NONE',  ( -0.000000000000000000, -0.000000000000000000, -1.000000000000000000 ) ) ;
#6420 = ORIENTED_EDGE ( 'NONE', *, *, #2088, .T. ) ;
#6421 = CIRCLE ( 'NONE', #506, 8.000000000000000000 ) ;
#6422 = DIRECTION ( 'NONE',  ( 0.000000000000000000, -0.9961946980917445460, -0.08715574274766943463 ) ) ;
#6423 = ADVANCED_FACE ( 'NONE', ( #2458 ), #5686, .T. ) ;
#6424 = ORIENTED_EDGE ( 'NONE', *, *, #554, .T. ) ;
#6425 = ORIENTED_EDGE ( 'NONE', *, *, #1306, .T. ) ;
#6426 = DIRECTION ( 'NONE',  ( 0.000000000000000000, 0.000000000000000000, 1.000000000000000000 ) ) ;
#6427 = LINE ( 'NONE', #5736, #3633 ) ;
#6428 =( BOUNDED_CURVE ( )  B_SPLINE_CURVE ( 3, ( #2198, #7084, #4532, #6331 ),
 .UNSPECIFIED., .F., .T. ) 
 B_SPLINE_CURVE_WITH_KNOTS ( ( 4, 4 ),
 ( 1.570796326794896558, 4.712388980384689674 ),
 .UNSPECIFIED. ) 
 CURVE ( )  GEOMETRIC_REPRESENTATION_ITEM ( )  RATIONAL_B_SPLINE_CURVE ( ( 1.000000000000000000, 0.3333333333333333703, 0.3333333333333333703, 1.000000000000000000 ) ) 
 REPRESENTATION_ITEM ( '' )  );
#6429 = CARTESIAN_POINT ( 'NONE',  ( -16.29350689640809691, -140.1746510883711778, -27.01918567566963247 ) ) ;
#6430 = EDGE_LOOP ( 'NONE', ( #3701, #7717, #8540 ) ) ;
#6431 = CARTESIAN_POINT ( 'NONE',  ( -2.293506896408097795, 42.08684478514406635, -25.00000000000000355 ) ) ;
#6432 = EDGE_CURVE ( 'NONE', #5197, #6817, #821, .T. ) ;
#6433 = EDGE_CURVE ( 'NONE', #4824, #8741, #8930, .T. ) ;
#6434 = EDGE_CURVE ( 'NONE', #1117, #4058, #1080, .T. ) ;
#6435 = ORIENTED_EDGE ( 'NONE', *, *, #4035, .T. ) ;
#6436 = CYLINDRICAL_SURFACE ( 'NONE', #2679, 5.000000000000000888 ) ;
#6437 = EDGE_LOOP ( 'NONE', ( #3712, #9205, #122, #3293 ) ) ;
#6438 = ORIENTED_EDGE ( 'NONE', *, *, #10418, .F. ) ;
#6439 = FACE_OUTER_BOUND ( 'NONE', #9587, .T. ) ;
#6440 = AXIS2_PLACEMENT_3D ( 'NONE', #4273, #3479, #4169 ) ;
#6441 = DIRECTION ( 'NONE',  ( 0.000000000000000000, -0.8660254037844394848, -0.4999999999999985567 ) ) ;
#6442 = CARTESIAN_POINT ( 'NONE',  ( -26.62179802177712773, -135.1457019118818721, -50.00000000000002132 ) ) ;
#6443 = DIRECTION ( 'NONE',  ( 1.000000000000000000, -0.000000000000000000, -0.000000000000000000 ) ) ;
#6444 = DIRECTION ( 'NONE',  ( -0.000000000000000000, 1.000000000000000000, -0.000000000000000000 ) ) ;
#6445 = PRODUCT_RELATED_PRODUCT_CATEGORY ( 'part', '', ( #3828 ) ) ;
#6446 = PRODUCT_DEFINITION_SHAPE ( 'NONE', 'NONE',  #10484 ) ;
#6447 = EDGE_CURVE ( 'NONE', #7344, #1239, #6474, .T. ) ;
#6448 = ORIENTED_EDGE ( 'NONE', *, *, #1243, .F. ) ;
#6449 = CIRCLE ( 'NONE', #8141, 2.000000000000001776 ) ;
#6450 = CARTESIAN_POINT ( 'NONE',  ( 39.99999999999997158, -135.1457019118818721, 49.99999999999997868 ) ) ;
#6451 =( GEOMETRIC_REPRESENTATION_CONTEXT ( 3 ) GLOBAL_UNCERTAINTY_ASSIGNED_CONTEXT ( ( #3457 ) ) GLOBAL_UNIT_ASSIGNED_CONTEXT ( ( #7613, #7561, #10106 ) ) REPRESENTATION_CONTEXT ( 'NONE', 'WORKASPACE' ) );
#6452 = ORIENTED_EDGE ( 'NONE', *, *, #6377, .T. ) ;
#6453 = DIRECTION ( 'NONE',  ( -1.000000000000000000, -0.000000000000000000, -0.000000000000000000 ) ) ;
#6454 = DIRECTION ( 'NONE',  ( 0.000000000000000000, 0.000000000000000000, 1.000000000000000000 ) ) ;
#6455 = DIRECTION ( 'NONE',  ( -0.000000000000000000, 1.000000000000000000, -0.000000000000000000 ) ) ;
#6456 = FACE_BOUND ( 'NONE', #9284, .T. ) ;
#6457 = CARTESIAN_POINT ( 'NONE',  ( -40.00000000000002842, -145.1457019118819005, 39.99999999999997868 ) ) ;
#6458 = VECTOR ( 'NONE', #10201, 1000.000000000000114 ) ;
#6459 = VECTOR ( 'NONE', #5244, 1000.000000000000000 ) ;
#6460 = EDGE_LOOP ( 'NONE', ( #9710, #1309, #7566, #5724 ) ) ;
#6461 = ORIENTED_EDGE ( 'NONE', *, *, #5966, .F. ) ;
#6462 = VERTEX_POINT ( 'NONE', #1187 ) ;
#6463 = AXIS2_PLACEMENT_3D ( 'NONE', #5917, #2899, #1102 ) ;
#6464 = ORIENTED_EDGE ( 'NONE', *, *, #7617, .F. ) ;
#6465 = AXIS2_PLACEMENT_3D ( 'NONE', #3798, #2999, #765 ) ;
#6466 = DIRECTION ( 'NONE',  ( -0.000000000000000000, 1.000000000000000000, -0.000000000000000000 ) ) ;
#6467 = EDGE_CURVE ( 'NONE', #490, #6578, #891, .T. ) ;
#6468 = CARTESIAN_POINT ( 'NONE',  ( -40.00000000000001421, -135.1457019118818721, -40.00000000000002132 ) ) ;
#6469 = LINE ( 'NONE', #5470, #8501 ) ;
#6470 = EDGE_LOOP ( 'NONE', ( #9327, #7472, #5174, #4278, #8267 ) ) ;
#6471 = CARTESIAN_POINT ( 'NONE',  ( 0.000000000000000000, -115.1457019118818863, 25.15769640663938134 ) ) ;
#6472 = VECTOR ( 'NONE', #7018, 1000.000000000000000 ) ;
#6473 = ORIENTED_EDGE ( 'NONE', *, *, #1683, .T. ) ;
#6474 = CIRCLE ( 'NONE', #3608, 4.000000000000000000 ) ;
#6475 = LINE ( 'NONE', #127, #8955 ) ;
#6476 = ORIENTED_EDGE ( 'NONE', *, *, #8123, .F. ) ;
#6477 = ORIENTED_EDGE ( 'NONE', *, *, #10407, .F. ) ;
#6478 = CARTESIAN_POINT ( 'NONE',  ( -50.00000000000002132, -135.1457019118818721, -6.938893903907231533E-15 ) ) ;
#6479 = AXIS2_PLACEMENT_3D ( 'NONE', #174, #1699, #1752 ) ;
#6480 = DIRECTION ( 'NONE',  ( 0.000000000000000000, -0.000000000000000000, -1.000000000000000000 ) ) ;
#6481 = EDGE_CURVE ( 'NONE', #3054, #7273, #3685, .T. ) ;
#6482 = DIRECTION ( 'NONE',  ( 0.000000000000000000, 0.000000000000000000, 1.000000000000000000 ) ) ;
#6483 = CARTESIAN_POINT ( 'NONE',  ( -47.94539818030328604, 85.52895752738115220, 0.000000000000000000 ) ) ;
#6484 = VERTEX_POINT ( 'NONE', #7705 ) ;
#6485 = CYLINDRICAL_SURFACE ( 'NONE', #5437, 5.000000000000000888 ) ;
#6486 = CIRCLE ( 'NONE', #7507, 2.541999999999999815 ) ;
#6487 = EDGE_LOOP ( 'NONE', ( #3275, #3528, #425, #1214 ) ) ;
#6488 = CIRCLE ( 'NONE', #9204, 5.000000000000000888 ) ;
#6489 = FACE_OUTER_BOUND ( 'NONE', #2168, .T. ) ;
#6490 = VERTEX_POINT ( 'NONE', #6915 ) ;
#6491 = ORIENTED_EDGE ( 'NONE', *, *, #4816, .F. ) ;
#6492 =( BOUNDED_CURVE ( )  B_SPLINE_CURVE ( 3, ( #3987, #1447, #7219, #8858 ),
 .UNSPECIFIED., .F., .T. ) 
 B_SPLINE_CURVE_WITH_KNOTS ( ( 4, 4 ),
 ( 2.243596561310088777, 4.039588745869492570 ),
 .UNSPECIFIED. ) 
 CURVE ( )  GEOMETRIC_REPRESENTATION_ITEM ( )  RATIONAL_B_SPLINE_CURVE ( ( 1.000000000000000000, 0.7487856226529291392, 0.7487856226529291392, 1.000000000000000000 ) ) 
 REPRESENTATION_ITEM ( '' )  );
#6493 = EDGE_CURVE ( 'NONE', #5509, #3393, #3522, .T. ) ;
#6494 = EDGE_CURVE ( 'NONE', #6206, #2621, #7836, .T. ) ;
#6495 = CARTESIAN_POINT ( 'NONE',  ( 4.856471286862176662, 145.0444252872335937, 30.00000000000000355 ) ) ;
#6496 = DIRECTION ( 'NONE',  ( -7.848480207562752404E-17, 1.000000000000000000, 0.000000000000000000 ) ) ;
#6497 = CIRCLE ( 'NONE', #5314, 4.999999999999995559 ) ;
#6498 = LINE ( 'NONE', #5807, #9851 ) ;
#6499 = DIRECTION ( 'NONE',  ( 0.000000000000000000, 0.000000000000000000, -1.000000000000000000 ) ) ;
#6500 = ORIENTED_EDGE ( 'NONE', *, *, #7804, .F. ) ;
#6501 = CIRCLE ( 'NONE', #1087, 10.00000000000000178 ) ;
#6502 = DIRECTION ( 'NONE',  ( 1.000000000000000000, 0.000000000000000000, 0.000000000000000000 ) ) ;
#6503 = VECTOR ( 'NONE', #522, 1000.000000000000000 ) ;
#6504 = ORIENTED_EDGE ( 'NONE', *, *, #5335, .T. ) ;
#6505 = CARTESIAN_POINT ( 'NONE',  ( -40.00000000000001421, -135.1707019118818778, -36.00000000000002842 ) ) ;
#6506 = EDGE_CURVE ( 'NONE', #8244, #1695, #8847, .T. ) ;
#6507 = DIRECTION ( 'NONE',  ( 1.000000000000000000, -0.000000000000000000, -0.000000000000000000 ) ) ;
#6508 = EDGE_CURVE ( 'NONE', #7051, #3749, #7652, .T. ) ;
#6509 = EDGE_CURVE ( 'NONE', #9955, #9452, #9998, .T. ) ;
#6510 = CARTESIAN_POINT ( 'NONE',  ( -23.17384457509314899, 150.5696653505793563, -10.90000000000000036 ) ) ;
#6511 = DIRECTION ( 'NONE',  ( -1.000000000000000000, -0.000000000000000000, -0.000000000000000000 ) ) ;
#6512 = AXIS2_PLACEMENT_3D ( 'NONE', #2230, #5711, #1898 ) ;
#6513 = FACE_OUTER_BOUND ( 'NONE', #8515, .T. ) ;
#6514 = VERTEX_POINT ( 'NONE', #7605 ) ;
#6515 = ORIENTED_EDGE ( 'NONE', *, *, #9660, .T. ) ;
#6516 = AXIS2_PLACEMENT_3D ( 'NONE', #8897, #5023, #269 ) ;
#6517 = ORIENTED_EDGE ( 'NONE', *, *, #1669, .F. ) ;
#6518 = ORIENTED_EDGE ( 'NONE', *, *, #9035, .F. ) ;
#6519 = DIRECTION ( 'NONE',  ( -1.000000000000000000, 0.000000000000000000, 0.000000000000000000 ) ) ;
#6520 = AXIS2_PLACEMENT_3D ( 'NONE', #7888, #629, #3869 ) ;
#6521 = ADVANCED_FACE ( 'NONE', ( #3628 ), #8445, .F. ) ;
#6522 = DIRECTION ( 'NONE',  ( 0.000000000000000000, -1.000000000000000000, 1.329743448921561232E-15 ) ) ;
#6523 = CARTESIAN_POINT ( 'NONE',  ( -47.94539818030330025, 90.52895752738122326, 0.000000000000000000 ) ) ;
#6524 = VERTEX_POINT ( 'NONE', #1980 ) ;
#6525 = CARTESIAN_POINT ( 'NONE',  ( -2.293506896408097795, -0.3998014571812398832, 1.076388538564875708 ) ) ;
#6526 = VECTOR ( 'NONE', #8232, 1000.000000000000000 ) ;
#6527 = ORIENTED_EDGE ( 'NONE', *, *, #5858, .T. ) ;
#6528 = PRESENTATION_STYLE_ASSIGNMENT (( #2394 ) ) ;
#6529 = EDGE_CURVE ( 'NONE', #9834, #10419, #4276, .T. ) ;
#6530 = CIRCLE ( 'NONE', #6018, 0.2500000000000002220 ) ;
#6531 = VERTEX_POINT ( 'NONE', #2673 ) ;
#6532 = UNCERTAINTY_MEASURE_WITH_UNIT (LENGTH_MEASURE( 1.000000000000000082E-05 ), #9441, 'distance_accuracy_value', 'NONE');
#6533 = ORIENTED_EDGE ( 'NONE', *, *, #6835, .F. ) ;
#6534 = DIRECTION ( 'NONE',  ( 0.000000000000000000, -1.000000000000000000, 0.000000000000000000 ) ) ;
#6535 = CARTESIAN_POINT ( 'NONE',  ( 67.68113203623319407, 150.5696653505793563, 10.98204862120179826 ) ) ;
#6536 = DIRECTION ( 'NONE',  ( -0.000000000000000000, 1.000000000000000000, -0.000000000000000000 ) ) ;
#6537 = DIRECTION ( 'NONE',  ( -0.6585271261848804070, 0.7525569905852197428, -0.000000000000000000 ) ) ;
#6538 = VECTOR ( 'NONE', #25, 1000.000000000000000 ) ;
#6539 = CARTESIAN_POINT ( 'NONE',  ( -16.29350689640809691, -8.660287962196477451, 0.000000000000000000 ) ) ;
#6540 = DIRECTION ( 'NONE',  ( 1.000000000000000000, 0.000000000000000000, 0.000000000000000000 ) ) ;
#6541 = ORIENTED_EDGE ( 'NONE', *, *, #1915, .F. ) ;
#6542 = DIRECTION ( 'NONE',  ( 1.000000000000000000, 0.000000000000000000, 0.000000000000000000 ) ) ;
#6543 = EDGE_CURVE ( 'NONE', #1670, #2698, #6449, .T. ) ;
#6544 = VECTOR ( 'NONE', #2026, 1000.000000000000000 ) ;
#6545 = ORIENTED_EDGE ( 'NONE', *, *, #6886, .T. ) ;
#6546 = DIRECTION ( 'NONE',  ( 0.000000000000000000, 0.000000000000000000, -1.000000000000000000 ) ) ;
#6547 = VECTOR ( 'NONE', #3692, 1000.000000000000000 ) ;
#6548 = EDGE_LOOP ( 'NONE', ( #1556, #6764, #8105, #5500 ) ) ;
#6549 = DIRECTION ( 'NONE',  ( 0.000000000000000000, 1.000000000000000000, 0.000000000000000000 ) ) ;
#6550 = CARTESIAN_POINT ( 'NONE',  ( -3.173844575093148990, 90.52895752738122326, 10.90000000000000036 ) ) ;
#6551 = CARTESIAN_POINT ( 'NONE',  ( 37.59878849545336976, 32.08684478514406635, -12.49999999999999289 ) ) ;
#6552 = DIRECTION ( 'NONE',  ( 0.000000000000000000, 0.000000000000000000, 1.000000000000000000 ) ) ;
#6553 = AXIS2_PLACEMENT_3D ( 'NONE', #4877, #2309, #5534 ) ;
#6554 = CARTESIAN_POINT ( 'NONE',  ( -56.36957570605427037, 137.0132282531173473, 4.025000000000000355 ) ) ;
#6555 = VERTEX_POINT ( 'NONE', #9193 ) ;
#6556 = EDGE_CURVE ( 'NONE', #84, #3945, #6059, .T. ) ;
#6557 = ADVANCED_FACE ( 'NONE', ( #4371 ), #4316, .F. ) ;
#6558 = ORIENTED_EDGE ( 'NONE', *, *, #8580, .F. ) ;
#6559 = AXIS2_PLACEMENT_3D ( 'NONE', #10414, #1457, #3999 ) ;
#6560 = PLANE ( 'NONE',  #958 ) ;
#6561 = SHAPE_REPRESENTATION ( 'Metal Mounting Block', ( #4601 ), #9214 ) ;
#6562 = ORIENTED_EDGE ( 'NONE', *, *, #4944, .F. ) ;
#6563 = CARTESIAN_POINT ( 'NONE',  ( -158.9246696254695337, 264.3597160760069187, 0.000000000000000000 ) ) ;
#6564 = DIRECTION ( 'NONE',  ( 0.000000000000000000, 1.734723475976809067E-15, 1.000000000000000000 ) ) ;
#6565 = CARTESIAN_POINT ( 'NONE',  ( -2.293506896408097795, 80.56966535057935630, -20.00000000000000711 ) ) ;
#6566 = DIRECTION ( 'NONE',  ( -1.000000000000000000, -0.000000000000000000, -0.000000000000000000 ) ) ;
#6567 = CYLINDRICAL_SURFACE ( 'NONE', #92, 2.000000000000001776 ) ;
#6568 = TOROIDAL_SURFACE ( 'NONE', #146, 4.700000000000000178, 0.2999999999999999889 ) ;
#6569 = CARTESIAN_POINT ( 'NONE',  ( 0.000000000000000000, 0.000000000000000000, 0.000000000000000000 ) ) ;
#6570 = ORIENTED_EDGE ( 'NONE', *, *, #8842, .F. ) ;
#6571 = ORIENTED_EDGE ( 'NONE', *, *, #2033, .T. ) ;
#6572 = EDGE_CURVE ( 'NONE', #7421, #7191, #5464, .T. ) ;
#6573 = EDGE_CURVE ( 'NONE', #4377, #34, #2504, .T. ) ;
#6574 = VERTEX_POINT ( 'NONE', #1875 ) ;
#6575 = EDGE_CURVE ( 'NONE', #3699, #4400, #8169, .T. ) ;
#6576 = AXIS2_PLACEMENT_3D ( 'NONE', #6251, #2281, #7157 ) ;
#6577 = ORIENTED_EDGE ( 'NONE', *, *, #9022, .F. ) ;
#6578 = VERTEX_POINT ( 'NONE', #3143 ) ;
#6579 = CARTESIAN_POINT ( 'NONE',  ( 67.68113203623319407, 65.56966535057937051, 10.98204862120179826 ) ) ;
#6580 = CARTESIAN_POINT ( 'NONE',  ( 37.59878849545336976, 32.08684478514406635, 12.50000000000000355 ) ) ;
#6581 = CARTESIAN_POINT ( 'NONE',  ( -16.29350689640809691, 11.33971203780352255, 0.000000000000000000 ) ) ;
#6582 = LINE ( 'NONE', #9065, #4364 ) ;
#6583 = EDGE_CURVE ( 'NONE', #5111, #6849, #5963, .T. ) ;
#6584 = ORIENTED_EDGE ( 'NONE', *, *, #7644, .T. ) ;
#6585 = DIRECTION ( 'NONE',  ( 1.000000000000000000, 0.000000000000000000, 0.000000000000000000 ) ) ;
#6586 = ORIENTED_EDGE ( 'NONE', *, *, #3348, .F. ) ;
#6587 = EDGE_CURVE ( 'NONE', #4136, #4219, #4113, .T. ) ;
#6588 = AXIS2_PLACEMENT_3D ( 'NONE', #4162, #144, #8292 ) ;
#6589 = ORIENTED_EDGE ( 'NONE', *, *, #9365, .F. ) ;
#6590 = CARTESIAN_POINT ( 'NONE',  ( -23.79350689640810401, 120.5289575273812233, 7.750000000000007105 ) ) ;
#6591 = DIRECTION ( 'NONE',  ( 1.000000000000000000, -0.000000000000000000, -0.000000000000000000 ) ) ;
#6592 = CIRCLE ( 'NONE', #2021, 3.999999999999989786 ) ;
#6593 = FACE_OUTER_BOUND ( 'NONE', #5835, .T. ) ;
#6594 = CARTESIAN_POINT ( 'NONE',  ( -30.29350689640809335, 37.08684478514406635, 0.000000000000000000 ) ) ;
#6595 = VERTEX_POINT ( 'NONE', #552 ) ;
#6596 = CARTESIAN_POINT ( 'NONE',  ( -30.29350689640809335, 80.56966535057935630, -24.00000000000000711 ) ) ;
#6597 = CONTEXT_DEPENDENT_SHAPE_REPRESENTATION ( #1114, #5602 ) ;
#6598 = EDGE_LOOP ( 'NONE', ( #4190, #6515, #7595, #9899 ) ) ;
#6599 = DIRECTION ( 'NONE',  ( 0.000000000000000000, 0.000000000000000000, 1.000000000000000000 ) ) ;
#6600 = VERTEX_POINT ( 'NONE', #2932 ) ;
#6601 =( NAMED_UNIT ( * ) PLANE_ANGLE_UNIT ( ) SI_UNIT ( $, .RADIAN. ) );
#6602 = EDGE_LOOP ( 'NONE', ( #9036, #2759 ) ) ;
#6603 = EDGE_CURVE ( 'NONE', #4826, #7421, #8708, .T. ) ;
#6604 = CARTESIAN_POINT ( 'NONE',  ( -48.00000000000002132, -115.1457019118818863, -25.15769640663945950 ) ) ;
#6605 = CARTESIAN_POINT ( 'NONE',  ( -2.293506896408101348, 42.08684478514406635, 25.00000000000000000 ) ) ;
#6606 = DIRECTION ( 'NONE',  ( -1.000000000000000000, 0.000000000000000000, 0.000000000000000000 ) ) ;
#6607 = CYLINDRICAL_SURFACE ( 'NONE', #7998, 4.729641367753004033 ) ;
#6608 = ORIENTED_EDGE ( 'NONE', *, *, #8049, .F. ) ;
#6609 = FACE_OUTER_BOUND ( 'NONE', #6161, .T. ) ;
#6610 = ORIENTED_EDGE ( 'NONE', *, *, #9035, .T. ) ;
#6611 = DIRECTION ( 'NONE',  ( -0.000000000000000000, 1.000000000000000000, -0.000000000000000000 ) ) ;
#6612 = CYLINDRICAL_SURFACE ( 'NONE', #204, 5.000000000000000888 ) ;
#6613 = DIRECTION ( 'NONE',  ( -9.101836848464095537E-17, -0.000000000000000000, -1.000000000000000000 ) ) ;
#6614 = DIRECTION ( 'NONE',  ( 0.000000000000000000, 1.000000000000000000, 0.000000000000000000 ) ) ;
#6615 = ADVANCED_FACE ( 'NONE', ( #7177 ), #6162, .F. ) ;
#6616 = CYLINDRICAL_SURFACE ( 'NONE', #2788, 2.000000000000001776 ) ;
#6617 = CARTESIAN_POINT ( 'NONE',  ( 27.15769640663938489, -133.1457019118818721, -27.15769640663940621 ) ) ;
#6618 = ORIENTED_EDGE ( 'NONE', *, *, #1949, .T. ) ;
#6619 = AXIS2_PLACEMENT_3D ( 'NONE', #8195, #5009, #6660 ) ;
#6620 = EDGE_LOOP ( 'NONE', ( #3542, #6518 ) ) ;
#6621 = ORIENTED_EDGE ( 'NONE', *, *, #4285, .T. ) ;
#6622 = DIRECTION ( 'NONE',  ( -0.7431448254773957984, 0.6691306063588565722, -0.000000000000000000 ) ) ;
#6623 = CARTESIAN_POINT ( 'NONE',  ( -2.293506896408097795, -3.651280424770854409E-15, 24.99999999999998579 ) ) ;
#6624 = AXIS2_PLACEMENT_3D ( 'NONE', #5657, #998, #8146 ) ;
#6625 = CIRCLE ( 'NONE', #2057, 6.499999999999964473 ) ;
#6626 = CARTESIAN_POINT ( 'NONE',  ( -30.29350689640809335, 2.445795361565304815E-15, 20.00000000000002132 ) ) ;
#6627 = EDGE_CURVE ( 'NONE', #9125, #10187, #1881, .T. ) ;
#6628 = DIRECTION ( 'NONE',  ( -1.000000000000000000, -0.000000000000000000, -0.000000000000000000 ) ) ;
#6629 = EDGE_CURVE ( 'NONE', #9495, #8325, #2299, .T. ) ;
#6630 = EDGE_CURVE ( 'NONE', #6085, #6356, #9402, .T. ) ;
#6631 = ORIENTED_EDGE ( 'NONE', *, *, #7347, .F. ) ;
#6632 = CARTESIAN_POINT ( 'NONE',  ( -38.96131932220313132, 3.319229491889295502, -2.232199717805805061 ) ) ;
#6633 = ORIENTED_EDGE ( 'NONE', *, *, #9769, .T. ) ;
#6634 = AXIS2_PLACEMENT_3D ( 'NONE', #5734, #7441, #9839 ) ;
#6635 = AXIS2_PLACEMENT_3D ( 'NONE', #1112, #6730, #9333 ) ;
#6636 = ORIENTED_EDGE ( 'NONE', *, *, #3733, .F. ) ;
#6637 = PRODUCT_DEFINITION_CONTEXT ( 'detailed design', #7882, 'design' ) ;
#6638 = DIRECTION ( 'NONE',  ( -0.6691306063588564612, -0.7431448254773957984, 0.000000000000000000 ) ) ;
#6639 = DIRECTION ( 'NONE',  ( 1.000000000000000000, -0.000000000000000000, -0.000000000000000000 ) ) ;
#6640 = CARTESIAN_POINT ( 'NONE',  ( -23.15769640663937423, -115.1457019118818863, -48.00000000000002132 ) ) ;
#6641 = CARTESIAN_POINT ( 'NONE',  ( -25.15769640663940976, -115.1457019118818863, 47.99999999999997868 ) ) ;
#6642 = EDGE_CURVE ( 'NONE', #2621, #6206, #4591, .T. ) ;
#6643 = CIRCLE ( 'NONE', #7834, 2.000000000000001776 ) ;
#6644 = EDGE_CURVE ( 'NONE', #4565, #36, #2137, .T. ) ;
#6645 = CIRCLE ( 'NONE', #5115, 3.999999999999996447 ) ;
#6646 = CARTESIAN_POINT ( 'NONE',  ( -24.29350689640808625, 140.5696653505793563, 10.98204862120179826 ) ) ;
#6647 = CARTESIAN_POINT ( 'NONE',  ( -3.173844575093148990, 90.52895752738122326, 10.90000000000000036 ) ) ;
#6648 = VERTEX_POINT ( 'NONE', #2250 ) ;
#6649 = CARTESIAN_POINT ( 'NONE',  ( 49.99999999999998579, -135.1457019118818721, -40.00000000000002132 ) ) ;
#6650 = ITEM_DEFINED_TRANSFORMATION ( 'NONE', 'NONE', #5815,  #4601 ) ;
#6651 = ORIENTED_EDGE ( 'NONE', *, *, #3008, .T. ) ;
#6652 = AXIS2_PLACEMENT_3D ( 'NONE', #9281, #3612, #2916 ) ;
#6653 = DIRECTION ( 'NONE',  ( 0.000000000000000000, 0.000000000000000000, 1.000000000000000000 ) ) ;
#6654 = ORIENTED_EDGE ( 'NONE', *, *, #401, .F. ) ;
#6655 = EDGE_CURVE ( 'NONE', #5226, #10069, #7921, .T. ) ;
#6656 = CARTESIAN_POINT ( 'NONE',  ( -30.29350689640809335, 2.445795361565304815E-15, -20.00000000000002132 ) ) ;
#6657 = CARTESIAN_POINT ( 'NONE',  ( 0.000000000000000000, -135.1457019118818721, 0.000000000000000000 ) ) ;
#6658 = FACE_OUTER_BOUND ( 'NONE', #10306, .T. ) ;
#6659 = AXIS2_PLACEMENT_3D ( 'NONE', #2694, #5921, #9323 ) ;
#6660 = DIRECTION ( 'NONE',  ( 0.000000000000000000, 0.000000000000000000, -1.000000000000000000 ) ) ;
#6661 = CARTESIAN_POINT ( 'NONE',  ( 23.15769640663940265, -117.1457019118819005, -48.00000000000002132 ) ) ;
#6662 = EDGE_CURVE ( 'NONE', #5577, #4058, #3758, .T. ) ;
#6663 = VERTEX_POINT ( 'NONE', #3091 ) ;
#6664 = DIRECTION ( 'NONE',  ( 0.000000000000000000, -0.3481865296036273372, 0.9374252720097653313 ) ) ;
#6665 = AXIS2_PLACEMENT_3D ( 'NONE', #9592, #10278, #2323 ) ;
#6666 = ORIENTED_EDGE ( 'NONE', *, *, #6572, .F. ) ;
#6667 = DIRECTION ( 'NONE',  ( 1.000000000000000000, -0.000000000000000000, -0.000000000000000000 ) ) ;
#6668 = DIRECTION ( 'NONE',  ( 1.000000000000000000, 0.000000000000000000, -0.000000000000000000 ) ) ;
#6669 = PRESENTATION_LAYER_ASSIGNMENT (  '', '', ( #9306 ) ) ;
#6670 = LINE ( 'NONE', #5708, #9557 ) ;
#6671 = FACE_OUTER_BOUND ( 'NONE', #4248, .T. ) ;
#6672 = DIRECTION ( 'NONE',  ( 1.000000000000000000, -0.000000000000000000, -0.000000000000000000 ) ) ;
#6673 = CIRCLE ( 'NONE', #2101, 4.000000000000000000 ) ;
#6674 = ORIENTED_EDGE ( 'NONE', *, *, #7719, .T. ) ;
#6675 = ORIENTED_EDGE ( 'NONE', *, *, #9151, .F. ) ;
#6676 = VECTOR ( 'NONE', #730, 1000.000000000000000 ) ;
#6677 = ORIENTED_EDGE ( 'NONE', *, *, #8525, .F. ) ;
#6678 = DIRECTION ( 'NONE',  ( 1.000000000000000000, -0.000000000000000000, 0.000000000000000000 ) ) ;
#6679 = CARTESIAN_POINT ( 'NONE',  ( -2.293506896408097795, 152.5696653505793279, 25.00000000000000000 ) ) ;
#6680 = VECTOR ( 'NONE', #7365, 1000.000000000000000 ) ;
#6681 = DIRECTION ( 'NONE',  ( -1.000000000000000000, 0.000000000000000000, 0.000000000000000000 ) ) ;
#6682 = DIRECTION ( 'NONE',  ( -0.000000000000000000, 1.000000000000000000, -0.000000000000000000 ) ) ;
#6683 = AXIS2_PLACEMENT_3D ( 'NONE', #9661, #7262, #6407 ) ;
#6684 = ORIENTED_EDGE ( 'NONE', *, *, #4779, .T. ) ;
#6685 = LINE ( 'NONE', #9986, #5187 ) ;
#6686 = ORIENTED_EDGE ( 'NONE', *, *, #6249, .F. ) ;
#6687 = ADVANCED_FACE ( 'NONE', ( #6327 ), #9572, .F. ) ;
#6688 = EDGE_LOOP ( 'NONE', ( #1295, #6338, #2043, #2447 ) ) ;
#6689 = CARTESIAN_POINT ( 'NONE',  ( -23.17384457509314899, 150.5696653505793563, 10.90000000000000036 ) ) ;
#6690 = LINE ( 'NONE', #1664, #5939 ) ;
#6691 = CYLINDRICAL_SURFACE ( 'NONE', #944, 3.999999999999989786 ) ;
#6692 = DIRECTION ( 'NONE',  ( -0.000000000000000000, -0.000000000000000000, -1.000000000000000000 ) ) ;
#6693 = DIRECTION ( 'NONE',  ( 0.000000000000000000, -1.000000000000000000, 0.000000000000000000 ) ) ;
#6694 = FACE_OUTER_BOUND ( 'NONE', #7313, .T. ) ;
#6695 = AXIS2_PLACEMENT_3D ( 'NONE', #6867, #6761, #1299 ) ;
#6696 = VERTEX_POINT ( 'NONE', #10255 ) ;
#6697 = DIRECTION ( 'NONE',  ( 0.000000000000000000, -1.000000000000000000, -9.100899318238089922E-17 ) ) ;
#6698 = EDGE_CURVE ( 'NONE', #10187, #9869, #6374, .T. ) ;
#6700 = EDGE_CURVE ( 'NONE', #9607, #3068, #5366, .T. ) ;
#6699 = VERTEX_POINT ( 'NONE', #9460 ) ;
#6701 = VECTOR ( 'NONE', #1206, 1000.000000000000000 ) ;
#6702 = ADVANCED_FACE ( 'NONE', ( #2350 ), #5262, .F. ) ;
#6703 = DIRECTION ( 'NONE',  ( 1.000000000000000000, -0.000000000000000000, -0.000000000000000000 ) ) ;
#6704 = ORIENTED_EDGE ( 'NONE', *, *, #46, .T. ) ;
#6705 = CIRCLE ( 'NONE', #2985, 4.025000000000000355 ) ;
#6706 =( NAMED_UNIT ( * ) SI_UNIT ( $, .STERADIAN. ) SOLID_ANGLE_UNIT ( ) );
#6707 = FACE_OUTER_BOUND ( 'NONE', #3959, .T. ) ;
#6708 = FACE_OUTER_BOUND ( 'NONE', #5765, .T. ) ;
#6709 = LINE ( 'NONE', #254, #2126 ) ;
#6710 = AXIS2_PLACEMENT_3D ( 'NONE', #6909, #5997, #7646 ) ;
#6711 = CARTESIAN_POINT ( 'NONE',  ( 39.99999999999998579, -135.1457019118818721, -35.97500000000002274 ) ) ;
#6712 = LINE ( 'NONE', #3584, #3090 ) ;
#6713 = DIRECTION ( 'NONE',  ( 1.000000000000000000, 0.000000000000000000, 0.000000000000000000 ) ) ;
#6714 = ORIENTED_EDGE ( 'NONE', *, *, #9660, .F. ) ;
#6715 = EDGE_CURVE ( 'NONE', #3675, #2182, #5447, .T. ) ;
#6716 = CARTESIAN_POINT ( 'NONE',  ( 42.22511195853868315, -135.1457019118818721, 30.00000000000000355 ) ) ;
#6717 = VECTOR ( 'NONE', #8996, 1000.000000000000000 ) ;
#6718 = ORIENTED_EDGE ( 'NONE', *, *, #805, .F. ) ;
#6719 = CARTESIAN_POINT ( 'NONE',  ( 17.97972049165455388, 17.84145331825995484, -25.00000000000000355 ) ) ;
#6720 = DIRECTION ( 'NONE',  ( 0.000000000000000000, 0.000000000000000000, 1.000000000000000000 ) ) ;
#6721 = AXIS2_PLACEMENT_3D ( 'NONE', #7611, #2726, #9251 ) ;
#6722 = DIRECTION ( 'NONE',  ( -1.000000000000000000, -0.000000000000000000, -0.000000000000000000 ) ) ;
#6723 = CARTESIAN_POINT ( 'NONE',  ( -40.00000000000002842, -135.1707019118818778, 39.99999999999997868 ) ) ;
#6724 = FACE_OUTER_BOUND ( 'NONE', #5108, .T. ) ;
#6725 = AXIS2_PLACEMENT_3D ( 'NONE', #2398, #9576, #8071 ) ;
#6726 = ORIENTED_EDGE ( 'NONE', *, *, #3658, .F. ) ;
#6727 = ORIENTED_EDGE ( 'NONE', *, *, #9489, .F. ) ;
#6728 = ORIENTED_EDGE ( 'NONE', *, *, #2161, .F. ) ;
#6729 = DIRECTION ( 'NONE',  ( 0.000000000000000000, 0.000000000000000000, 1.000000000000000000 ) ) ;
#6730 = DIRECTION ( 'NONE',  ( -1.000000000000000000, -0.000000000000000000, -0.000000000000000000 ) ) ;
#6731 = CIRCLE ( 'NONE', #9795, 2.541999999999999815 ) ;
#6732 = CIRCLE ( 'NONE', #8254, 4.000000000000016875 ) ;
#6733 =( REPRESENTATION_RELATIONSHIP ('NONE','NONE', #9007, #3996 ) REPRESENTATION_RELATIONSHIP_WITH_TRANSFORMATION ( #5797 )SHAPE_REPRESENTATION_RELATIONSHIP( ) );
#6734 = DIRECTION ( 'NONE',  ( -1.000000000000000000, -0.000000000000000000, -0.000000000000000000 ) ) ;
#6735 = EDGE_CURVE ( 'NONE', #1811, #2339, #1725, .T. ) ;
#6736 = DIRECTION ( 'NONE',  ( 0.000000000000000000, 0.000000000000000000, 1.000000000000000000 ) ) ;
#6737 = EDGE_LOOP ( 'NONE', ( #99, #6892, #1109, #8343 ) ) ;
#6738 = DIRECTION ( 'NONE',  ( 0.000000000000000000, 0.000000000000000000, 1.000000000000000000 ) ) ;
#6739 = ORIENTED_EDGE ( 'NONE', *, *, #9503, .T. ) ;
#6740 = CARTESIAN_POINT ( 'NONE',  ( 3.000000000000000000, -1.467624384280032279, -2.541999999999998039 ) ) ;
#6741 = CIRCLE ( 'NONE', #2176, 4.000000000000016875 ) ;
#6742 = ORIENTED_EDGE ( 'NONE', *, *, #2032, .T. ) ;
#6743 = CARTESIAN_POINT ( 'NONE',  ( 26.00000000000000355, 0.000000000000000000, 0.000000000000000000 ) ) ;
#6744 = SURFACE_STYLE_USAGE ( .BOTH. , #291 ) ;
#6745 = LINE ( 'NONE', #7440, #5511 ) ;
#6746 = CARTESIAN_POINT ( 'NONE',  ( 73.53765631853929108, 70.39106037767955115, -25.00000000000000355 ) ) ;
#6747 = DIRECTION ( 'NONE',  ( -8.194486552889013533E-17, -9.100899318238110877E-17, 1.000000000000000000 ) ) ;
#6748 = EDGE_CURVE ( 'NONE', #5730, #596, #8485, .T. ) ;
#6749 = DIRECTION ( 'NONE',  ( 0.000000000000000000, 0.000000000000000000, 1.000000000000000000 ) ) ;
#6750 = ORIENTED_EDGE ( 'NONE', *, *, #5473, .F. ) ;
#6751 = VECTOR ( 'NONE', #3241, 1000.000000000000000 ) ;
#6752 = CARTESIAN_POINT ( 'NONE',  ( -30.29350689640809335, 80.56966535057935630, -20.00000000000000711 ) ) ;
#6753 = VERTEX_POINT ( 'NONE', #8796 ) ;
#6754 = CARTESIAN_POINT ( 'NONE',  ( -50.00000000000002842, -115.1457019118818863, 39.99999999999997868 ) ) ;
#6755 = EDGE_LOOP ( 'NONE', ( #5739, #2123, #4041, #4493 ) ) ;
#6756 = SHAPE_REPRESENTATION_RELATIONSHIP ( 'NONE' , 'NONE' ,  #9697, #9745 ) ;
#6757 = DIRECTION ( 'NONE',  ( 0.000000000000000000, 0.000000000000000000, -1.000000000000000000 ) ) ;
#6758 = DIRECTION ( 'NONE',  ( 0.1124875939035005212, 0.8191520442889906883, 0.5624379695175003580 ) ) ;
#6759 = EDGE_CURVE ( 'NONE', #2974, #3710, #707, .T. ) ;
#6760 = EDGE_CURVE ( 'NONE', #2186, #7029, #2282, .T. ) ;
#6761 = DIRECTION ( 'NONE',  ( 1.000000000000000000, 0.000000000000000000, 9.776117811460147207E-16 ) ) ;
#6762 = ADVANCED_FACE ( 'NONE', ( #6252, #2225, #6197 ), #4607, .F. ) ;
#6763 = LINE ( 'NONE', #6811, #1384 ) ;
#6764 = ORIENTED_EDGE ( 'NONE', *, *, #3194, .T. ) ;
#6765 = CARTESIAN_POINT ( 'NONE',  ( -2.293506896408097795, 120.5696653505793705, -16.00000000000000711 ) ) ;
#6766 = DIRECTION ( 'NONE',  ( 1.000000000000000000, 0.000000000000000000, 0.000000000000000000 ) ) ;
#6767 = ORIENTED_EDGE ( 'NONE', *, *, #7033, .T. ) ;
#6768 = CARTESIAN_POINT ( 'NONE',  ( 53.40242741783141156, 52.77167129626698028, 25.00000000000000000 ) ) ;
#6769 = ORIENTED_EDGE ( 'NONE', *, *, #2429, .T. ) ;
#6770 = DIRECTION ( 'NONE',  ( 6.106226635438360972E-16, -1.000000000000000000, 0.000000000000000000 ) ) ;
#6771 = DIRECTION ( 'NONE',  ( 0.000000000000000000, -0.000000000000000000, 1.000000000000000000 ) ) ;
#6772 = CARTESIAN_POINT ( 'NONE',  ( -2.293506896408097795, 0.000000000000000000, -10.98204862120179826 ) ) ;
#6773 = PRODUCT_DEFINITION ( 'UNKNOWN', '', #4471, #1020 ) ;
#6774 = DIRECTION ( 'NONE',  ( -0.000000000000000000, -0.000000000000000000, 1.000000000000000000 ) ) ;
#6775 = EDGE_CURVE ( 'NONE', #4450, #6524, #6799, .T. ) ;
#6776 = DIRECTION ( 'NONE',  ( -1.000000000000000000, 0.000000000000000000, 1.734723475976804383E-16 ) ) ;
#6777 = ORIENTED_EDGE ( 'NONE', *, *, #6956, .F. ) ;
#6778 = ORIENTED_EDGE ( 'NONE', *, *, #10013, .F. ) ;
#6779 = EDGE_LOOP ( 'NONE', ( #5898, #9164, #6541, #8356 ) ) ;
#6780 = CARTESIAN_POINT ( 'NONE',  ( -16.29350689640809691, 105.5289575273812233, 7.750000000000000000 ) ) ;
#6781 = CARTESIAN_POINT ( 'NONE',  ( -16.29350689640809691, -8.660287962196477451, 5.025000000000002132 ) ) ;
#6782 = CARTESIAN_POINT ( 'NONE',  ( -50.00000000000002132, -133.6308916829187581, 23.64290342185648797 ) ) ;
#6783 = PLANE ( 'NONE',  #2331 ) ;
#6784 = VECTOR ( 'NONE', #2904, 1000.000000000000114 ) ;
#6785 = ORIENTED_EDGE ( 'NONE', *, *, #3566, .T. ) ;
#6786 = CARTESIAN_POINT ( 'NONE',  ( -50.00000000000002132, -117.1457019118819005, -6.938893903907231533E-15 ) ) ;
#6787 = ORIENTED_EDGE ( 'NONE', *, *, #2859, .T. ) ;
#6788 = FACE_OUTER_BOUND ( 'NONE', #10149, .T. ) ;
#6789 = EDGE_CURVE ( 'NONE', #1658, #1605, #6971, .T. ) ;
#6790 = AXIS2_PLACEMENT_3D ( 'NONE', #6106, #2827, #9350 ) ;
#6791 = APPLICATION_CONTEXT ( 'automotive_design' ) ;
#6792 = ORIENTED_EDGE ( 'NONE', *, *, #1709, .T. ) ;
#6793 = MECHANICAL_DESIGN_GEOMETRIC_PRESENTATION_REPRESENTATION (  '', ( #866 ), #2388 ) ;
#6794 = CARTESIAN_POINT ( 'NONE',  ( -47.94539818030330025, 137.0132282531173473, 3.999999999999991562 ) ) ;
#6795 = CARTESIAN_POINT ( 'NONE',  ( -25.15769640663940265, -133.1457019118818721, -3.513494341946491635E-15 ) ) ;
#6796 = CARTESIAN_POINT ( 'NONE',  ( -25.15769640663938134, -115.1457019118818863, -48.00000000000002132 ) ) ;
#6797 = CARTESIAN_POINT ( 'NONE',  ( -16.29350689640809691, 11.33971203780352255, 4.999999999999993783 ) ) ;
#6798 = LINE ( 'NONE', #10039, #9598 ) ;
#6799 = CIRCLE ( 'NONE', #2734, 4.295524112943372330 ) ;
#6800 = ORIENTED_EDGE ( 'NONE', *, *, #6789, .T. ) ;
#6801 = DIRECTION ( 'NONE',  ( 1.000000000000000000, 0.000000000000000000, -0.000000000000000000 ) ) ;
#6802 = ORIENTED_EDGE ( 'NONE', *, *, #2859, .F. ) ;
#6803 = FACE_OUTER_BOUND ( 'NONE', #3433, .T. ) ;
#6804 = EDGE_CURVE ( 'NONE', #2451, #288, #10237, .T. ) ;
#6805 = DIRECTION ( 'NONE',  ( -0.000000000000000000, 1.000000000000000000, -0.000000000000000000 ) ) ;
#6806 = AXIS2_PLACEMENT_3D ( 'NONE', #1893, #6022, #1260 ) ;
#6807 = AXIS2_PLACEMENT_3D ( 'NONE', #7353, #153, #5010 ) ;
#6808 = CARTESIAN_POINT ( 'NONE',  ( -20.29350689640810046, 150.5696653505793563, 20.00000000000000355 ) ) ;
#6809 = DIRECTION ( 'NONE',  ( 0.000000000000000000, 0.000000000000000000, 1.000000000000000000 ) ) ;
#6810 = DIRECTION ( 'NONE',  ( 0.000000000000000000, 0.000000000000000000, 1.000000000000000000 ) ) ;
#6811 = CARTESIAN_POINT ( 'NONE',  ( -39.00428932080996702, 3.065011249696406370, -1.804608920635871749 ) ) ;
#6812 = ORIENTED_EDGE ( 'NONE', *, *, #2762, .F. ) ;
#6813 = DIRECTION ( 'NONE',  ( 0.000000000000000000, -1.000000000000000000, 0.000000000000000000 ) ) ;
#6814 = TOROIDAL_SURFACE ( 'NONE', #9541, -49.75669024694125397, 59.51479730733485951 ) ;
#6815 = VECTOR ( 'NONE', #9844, 1000.000000000000000 ) ;
#6816 = ORIENTED_EDGE ( 'NONE', *, *, #2489, .F. ) ;
#6817 = VERTEX_POINT ( 'NONE', #8743 ) ;
#6818 = CARTESIAN_POINT ( 'NONE',  ( 10.51964330236497602, 150.0000000000000000, -24.99999999999998934 ) ) ;
#6819 = ADVANCED_FACE ( 'NONE', ( #8689 ), #6301, .T. ) ;
#6820 = EDGE_CURVE ( 'NONE', #7406, #34, #4662, .T. ) ;
#6821 = MANIFOLD_SOLID_BREP ( 'Hex', #1650 ) ;
#6822 = EDGE_LOOP ( 'NONE', ( #1016, #3500, #2023, #8555 ) ) ;
#6823 = DIRECTION ( 'NONE',  ( 0.000000000000000000, 0.000000000000000000, 1.000000000000000000 ) ) ;
#6824 = CARTESIAN_POINT ( 'NONE',  ( 10.26554134690924691, 64.37996872128307757, -7.750000000000000000 ) ) ;
#6825 = ADVANCED_BREP_SHAPE_REPRESENTATION ( '', ( #6821, #4601 ), #3113 ) ;
#6826 = AXIS2_PLACEMENT_3D ( 'NONE', #4293, #6734, #278 ) ;
#6827 = CARTESIAN_POINT ( 'NONE',  ( -40.00000000000002842, -135.1457019118818721, 39.99999999999997868 ) ) ;
#6828 = CARTESIAN_POINT ( 'NONE',  ( -117.0000000000000000, 0.000000000000000000, 0.000000000000000000 ) ) ;
#6829 = LINE ( 'NONE', #6939, #6503 ) ;
#6830 = CARTESIAN_POINT ( 'NONE',  ( -48.00000000000002132, -133.1457019118818721, 25.15769640663938134 ) ) ;
#6831 = ORIENTED_EDGE ( 'NONE', *, *, #240, .F. ) ;
#6832 = EDGE_LOOP ( 'NONE', ( #7107, #3295, #1216, #3792, #4995, #4711, #3104 ) ) ;
#6833 = AXIS2_PLACEMENT_3D ( 'NONE', #1741, #4965, #9376 ) ;
#6834 = CARTESIAN_POINT ( 'NONE',  ( -30.29350689640809335, 120.5696653505793705, -20.00000000000000711 ) ) ;
#6835 = EDGE_CURVE ( 'NONE', #1563, #5352, #6295, .T. ) ;
#6836 = ADVANCED_FACE ( 'NONE', ( #7002 ), #7640, .T. ) ;
#6837 = ADVANCED_FACE ( 'NONE', ( #9440 ), #7814, .T. ) ;
#6838 = LINE ( 'NONE', #7527, #6062 ) ;
#6839 = CARTESIAN_POINT ( 'NONE',  ( -117.0000000000000000, 0.000000000000000000, 4.000000000000000000 ) ) ;
#6840 = DIRECTION ( 'NONE',  ( -1.000000000000000000, 0.000000000000000000, 0.000000000000000000 ) ) ;
#6841 =( BOUNDED_CURVE ( )  B_SPLINE_CURVE ( 3, ( #460, #310, #6868, #4383 ),
 .UNSPECIFIED., .F., .T. ) 
 B_SPLINE_CURVE_WITH_KNOTS ( ( 4, 4 ),
 ( 0.9691135948774319830, 1.037548729184187390 ),
 .UNSPECIFIED. ) 
 CURVE ( )  GEOMETRIC_REPRESENTATION_ITEM ( )  RATIONAL_B_SPLINE_CURVE ( ( 1.000000000000000000, 0.9996097574442918132, 0.9996097574442918132, 1.000000000000000000 ) ) 
 REPRESENTATION_ITEM ( '' )  );
#6842 = CARTESIAN_POINT ( 'NONE',  ( -2.293506896408097795, 120.5696653505793705, 16.00000000000000711 ) ) ;
#6843 = AXIS2_PLACEMENT_3D ( 'NONE', #1781, #8939, #199 ) ;
#6844 = ORIENTED_EDGE ( 'NONE', *, *, #3265, .F. ) ;
#6845 = CARTESIAN_POINT ( 'NONE',  ( -16.29350689640809691, 65.65569765742554864, 7.499999999999996447 ) ) ;
#6846 = VERTEX_POINT ( 'NONE', #7462 ) ;
#6847 = LINE ( 'NONE', #5249, #1348 ) ;
#6848 = VECTOR ( 'NONE', #6225, 1000.000000000000000 ) ;
#6849 = VERTEX_POINT ( 'NONE', #3435 ) ;
#6850 = EDGE_CURVE ( 'NONE', #2017, #2630, #8043, .T. ) ;
#6851 = CYLINDRICAL_SURFACE ( 'NONE', #2502, 4.000000000000000000 ) ;
#6852 = CARTESIAN_POINT ( 'NONE',  ( -47.94539818030330025, 137.0132282531173473, -3.999999999999991562 ) ) ;
#6853 = DIRECTION ( 'NONE',  ( 0.000000000000000000, 0.000000000000000000, 1.000000000000000000 ) ) ;
#6854 = CARTESIAN_POINT ( 'NONE',  ( -2.293506896408097795, 80.56966535057935630, 24.00000000000000711 ) ) ;
#6855 = ADVANCED_FACE ( 'NONE', ( #209 ), #10478, .T. ) ;
#6856 = CARTESIAN_POINT ( 'NONE',  ( 37.22759939293836595, -133.1457019118818721, -25.15769640663939910 ) ) ;
#6857 = AXIS2_PLACEMENT_3D ( 'NONE', #4030, #7263, #10446 ) ;
#6858 = ORIENTED_EDGE ( 'NONE', *, *, #1128, .T. ) ;
#6859 = DIRECTION ( 'NONE',  ( 0.000000000000000000, 0.000000000000000000, 1.000000000000000000 ) ) ;
#6860 = AXIS2_PLACEMENT_3D ( 'NONE', #8991, #9907, #7402 ) ;
#6861 = LINE ( 'NONE', #8554, #2352 ) ;
#6862 = CARTESIAN_POINT ( 'NONE',  ( 23.15769640663936713, -133.1457019118818721, 49.99999999999997868 ) ) ;
#6863 = AXIS2_PLACEMENT_3D ( 'NONE', #5223, #8506, #5166 ) ;
#6864 = CYLINDRICAL_SURFACE ( 'NONE', #1814, 7.999999999999994671 ) ;
#6865 = DIRECTION ( 'NONE',  ( -0.000000000000000000, 1.000000000000000000, -0.000000000000000000 ) ) ;
#6866 = EDGE_CURVE ( 'NONE', #5250, #7894, #4600, .T. ) ;
#6867 = CARTESIAN_POINT ( 'NONE',  ( 25.15769640663935292, -115.1457019118818863, 2.459446039362539254E-14 ) ) ;
#6868 = CARTESIAN_POINT ( 'NONE',  ( -39.65557114539780770, -3.370159726842522296, -2.156467633200152001 ) ) ;
#6869 = VERTEX_POINT ( 'NONE', #4128 ) ;
#6870 = CARTESIAN_POINT ( 'NONE',  ( 14.70649310359190309, 120.5696653505793705, -20.00000000000000711 ) ) ;
#6871 = VECTOR ( 'NONE', #1869, 1000.000000000000000 ) ;
#6872 = EDGE_LOOP ( 'NONE', ( #8288, #5960, #6047, #7479 ) ) ;
#6873 = ORIENTED_EDGE ( 'NONE', *, *, #3096, .T. ) ;
#6874 = AXIS2_PLACEMENT_3D ( 'NONE', #8455, #2729, #6810 ) ;
#6875 = DIRECTION ( 'NONE',  ( 1.000000000000000000, -0.000000000000000000, -0.000000000000000000 ) ) ;
#6876 = ORIENTED_EDGE ( 'NONE', *, *, #8261, .T. ) ;
#6877 = ORIENTED_EDGE ( 'NONE', *, *, #1053, .F. ) ;
#6878 = CYLINDRICAL_SURFACE ( 'NONE', #990, 10.00000000000000178 ) ;
#6879 = PLANE ( 'NONE',  #2906 ) ;
#6880 = TOROIDAL_SURFACE ( 'NONE', #9602, -49.75669024694125397, 59.51479730733485951 ) ;
#6881 = LINE ( 'NONE', #4494, #1851 ) ;
#6882 = DIRECTION ( 'NONE',  ( -0.000000000000000000, -0.000000000000000000, 1.000000000000000000 ) ) ;
#6883 = CARTESIAN_POINT ( 'NONE',  ( 67.68113203623319407, 65.56966535057937051, -10.98204862120179826 ) ) ;
#6884 = VECTOR ( 'NONE', #1449, 1000.000000000000000 ) ;
#6885 = CARTESIAN_POINT ( 'NONE',  ( 39.99999999999997158, -135.1457019118818721, 39.99999999999997868 ) ) ;
#6886 = EDGE_CURVE ( 'NONE', #5017, #979, #37, .T. ) ;
#6887 = EDGE_LOOP ( 'NONE', ( #2220, #2856 ) ) ;
#6888 = ORIENTED_EDGE ( 'NONE', *, *, #9935, .F. ) ;
#6889 = AXIS2_PLACEMENT_3D ( 'NONE', #6768, #7512, #262 ) ;
#6890 = DIRECTION ( 'NONE',  ( -0.000000000000000000, 1.000000000000000000, -0.000000000000000000 ) ) ;
#6891 = VECTOR ( 'NONE', #610, 1000.000000000000000 ) ;
#6892 = ORIENTED_EDGE ( 'NONE', *, *, #8084, .F. ) ;
#6893 = CARTESIAN_POINT ( 'NONE',  ( -48.00000000000002132, -117.1457019118819005, -23.15769640663945594 ) ) ;
#6894 =( LENGTH_UNIT ( ) NAMED_UNIT ( * ) SI_UNIT ( .MILLI., .METRE. ) );
#6895 = CARTESIAN_POINT ( 'NONE',  ( 23.15769640663936713, -115.1457019118818863, 47.99999999999997868 ) ) ;
#6896 = DIRECTION ( 'NONE',  ( 1.000000000000000000, 0.000000000000000000, -0.000000000000000000 ) ) ;
#6897 = ORIENTED_EDGE ( 'NONE', *, *, #4977, .T. ) ;
#6898 = ADVANCED_FACE ( 'NONE', ( #2532, #9702, #9917 ), #8259, .F. ) ;
#6899 = ADVANCED_FACE ( 'NONE', ( #8205 ), #102, .T. ) ;
#6900 = EDGE_CURVE ( 'NONE', #4047, #9459, #943, .T. ) ;
#6901 = ORIENTED_EDGE ( 'NONE', *, *, #2200, .T. ) ;
#6902 = CONICAL_SURFACE ( 'NONE', #5703, 4.025000000000000355, 0.7853981633975870569 ) ;
#6903 = EDGE_LOOP ( 'NONE', ( #1450, #1180, #9624 ) ) ;
#6904 = ORIENTED_EDGE ( 'NONE', *, *, #10340, .T. ) ;
#6905 = SHAPE_REPRESENTATION ( 'groove pin 01_iso_ISO 8739-M8x45-St', ( #4601 ), #1084 ) ;
#6906 = ORIENTED_EDGE ( 'NONE', *, *, #4374, .T. ) ;
#6907 = DIRECTION ( 'NONE',  ( 1.000000000000000000, 0.000000000000000000, 0.000000000000000000 ) ) ;
#6908 = DIRECTION ( 'NONE',  ( 0.000000000000000000, 0.000000000000000000, 1.000000000000000000 ) ) ;
#6909 = CARTESIAN_POINT ( 'NONE',  ( -121.7299640054770578, 230.8694527092982867, 0.000000000000000000 ) ) ;
#6910 = DIRECTION ( 'NONE',  ( 0.7525569905852205199, 0.6585271261848794078, 0.000000000000000000 ) ) ;
#6911 = PLANE ( 'NONE',  #4836 ) ;
#6912 = CIRCLE ( 'NONE', #9631, 5.000000000000007994 ) ;
#6913 = EDGE_CURVE ( 'NONE', #4137, #9125, #7143, .T. ) ;
#6914 = ORIENTED_EDGE ( 'NONE', *, *, #3925, .T. ) ;
#6915 = CARTESIAN_POINT ( 'NONE',  ( -30.29350689640809335, 55.56966535057937051, -10.98204862120179826 ) ) ;
#6916 = AXIS2_PLACEMENT_3D ( 'NONE', #1616, #4843, #672 ) ;
#6917 = DIRECTION ( 'NONE',  ( -0.000000000000000000, -1.000000000000000000, -0.000000000000000000 ) ) ;
#6918 = ORIENTED_EDGE ( 'NONE', *, *, #1293, .T. ) ;
#6919 = CIRCLE ( 'NONE', #1288, 19.24539146688411506 ) ;
#6920 = CARTESIAN_POINT ( 'NONE',  ( -25.15769640663937423, -133.1457019118818721, -48.00000000000002132 ) ) ;
#6921 = AXIS2_PLACEMENT_3D ( 'NONE', #8608, #2139, #453 ) ;
#6922 = DIRECTION ( 'NONE',  ( 9.776117811460147207E-16, 0.000000000000000000, -1.000000000000000000 ) ) ;
#6923 = FACE_OUTER_BOUND ( 'NONE', #10215, .T. ) ;
#6924 = FACE_OUTER_BOUND ( 'NONE', #2380, .T. ) ;
#6925 = ORIENTED_EDGE ( 'NONE', *, *, #8049, .T. ) ;
#6926 = DIRECTION ( 'NONE',  ( 0.000000000000000000, 0.000000000000000000, 1.000000000000000000 ) ) ;
#6927 = VERTEX_POINT ( 'NONE', #4178 ) ;
#6928 = VERTEX_POINT ( 'NONE', #8949 ) ;
#6929 = CARTESIAN_POINT ( 'NONE',  ( -168.7559887226705087, 267.8293446334839700, 0.000000000000000000 ) ) ;
#6930 = COLOUR_RGB ( '',0.7921568627450980005, 0.8196078431372548767, 0.9333333333333333481 ) ;
#6931 = ORIENTED_EDGE ( 'NONE', *, *, #5070, .T. ) ;
#6932 = EDGE_CURVE ( 'NONE', #6072, #6943, #2055, .T. ) ;
#6933 = VERTEX_POINT ( 'NONE', #7258 ) ;
#6934 = CARTESIAN_POINT ( 'NONE',  ( -147.2606667696710474, 253.8574007319445229, 0.000000000000000000 ) ) ;
#6935 = CARTESIAN_POINT ( 'NONE',  ( 3.000000000000000000, 0.000000000000000000, 0.000000000000000000 ) ) ;
#6936 = ORIENTED_EDGE ( 'NONE', *, *, #4309, .T. ) ;
#6937 = DIRECTION ( 'NONE',  ( 0.000000000000000000, 0.000000000000000000, 1.000000000000000000 ) ) ;
#6938 = DIRECTION ( 'NONE',  ( 0.000000000000000000, -0.4999999999999985012, 0.8660254037844393737 ) ) ;
#6939 = CARTESIAN_POINT ( 'NONE',  ( 14.70649310359190309, 80.56966535057935630, 16.00000000000000711 ) ) ;
#6940 = CARTESIAN_POINT ( 'NONE',  ( 0.000000000000000000, 0.000000000000000000, 10.90000000000000036 ) ) ;
#6941=STYLED_ITEM('',(#10518),#3318);
#6942 = ORIENTED_EDGE ( 'NONE', *, *, #2031, .T. ) ;
#6943 = VERTEX_POINT ( 'NONE', #7414 ) ;
#6944 = DIRECTION ( 'NONE',  ( 0.000000000000000000, 1.000000000000000000, 0.000000000000000000 ) ) ;
#6945 = VERTEX_POINT ( 'NONE', #4807 ) ;
#6946 = ADVANCED_FACE ( 'NONE', ( #161 ), #6612, .T. ) ;
#6947 = CARTESIAN_POINT ( 'NONE',  ( 59.99999999999999289, -135.1457019118818721, -30.00000000000000355 ) ) ;
#6948 = DIRECTION ( 'NONE',  ( 1.000000000000000000, 0.000000000000000000, 0.000000000000000000 ) ) ;
#6949 = CARTESIAN_POINT ( 'NONE',  ( -141.9789400531797412, 249.1017126355397977, 0.000000000000000000 ) ) ;
#6950 = CARTESIAN_POINT ( 'NONE',  ( -8.000000000000000000, -1.691446717414637702, 1.184363742013801124 ) ) ;
#6951 = DIRECTION ( 'NONE',  ( 0.000000000000000000, 0.000000000000000000, -1.000000000000000000 ) ) ;
#6952 = ORIENTED_EDGE ( 'NONE', *, *, #3494, .F. ) ;
#6953 = EDGE_LOOP ( 'NONE', ( #5764, #5134, #635, #1962 ) ) ;
#6954 = ORIENTED_EDGE ( 'NONE', *, *, #10283, .T. ) ;
#6955 = ORIENTED_EDGE ( 'NONE', *, *, #7290, .F. ) ;
#6956 = EDGE_CURVE ( 'NONE', #3747, #1040, #2588, .T. ) ;
#6957 = CARTESIAN_POINT ( 'NONE',  ( -40.00000000000002842, -135.1457019118818721, 35.99999999999999289 ) ) ;
#6958 = DIRECTION ( 'NONE',  ( -1.000000000000000000, -0.000000000000000000, 0.000000000000000000 ) ) ;
#6959 = EDGE_CURVE ( 'NONE', #2709, #9023, #5865, .T. ) ;
#6960 = AXIS2_PLACEMENT_3D ( 'NONE', #1624, #9801, #3270 ) ;
#6961 = DIRECTION ( 'NONE',  ( 0.000000000000000000, -1.000000000000000000, 0.000000000000000000 ) ) ;
#6962 = DIRECTION ( 'NONE',  ( 1.000000000000000000, -0.000000000000000000, -0.000000000000000000 ) ) ;
#6963 = FACE_OUTER_BOUND ( 'NONE', #8433, .T. ) ;
#6964 = ORIENTED_EDGE ( 'NONE', *, *, #7290, .T. ) ;
#6965 = DIRECTION ( 'NONE',  ( 0.000000000000000000, 0.000000000000000000, 1.000000000000000000 ) ) ;
#6966 = FACE_OUTER_BOUND ( 'NONE', #8140, .T. ) ;
#6967 = ADVANCED_FACE ( 'NONE', ( #7306 ), #51, .F. ) ;
#6968 = DIRECTION ( 'NONE',  ( 1.396588258780021135E-16, 0.000000000000000000, 1.000000000000000000 ) ) ;
#6969 = ADVANCED_FACE ( 'NONE', ( #2478 ), #6879, .F. ) ;
#6970 = ADVANCED_FACE ( 'NONE', ( #8416 ), #6078, .T. ) ;
#6971 = CIRCLE ( 'NONE', #538, 4.000000000000000000 ) ;
#6972 = CARTESIAN_POINT ( 'NONE',  ( -16.26850689640809478, 140.5696653505793563, 20.00000000000002132 ) ) ;
#6973 = MECHANICAL_DESIGN_GEOMETRIC_PRESENTATION_REPRESENTATION (  '', ( #3416 ), #9687 ) ;
#6974 = DIRECTION ( 'NONE',  ( -1.734723475976805319E-15, 0.000000000000000000, 1.000000000000000000 ) ) ;
#6975 = DIRECTION ( 'NONE',  ( 0.000000000000000000, 0.000000000000000000, 1.000000000000000000 ) ) ;
#6976 = ORIENTED_EDGE ( 'NONE', *, *, #2547, .T. ) ;
#6977 = CARTESIAN_POINT ( 'NONE',  ( 37.59878849545336976, 32.08684478514406635, 30.00000000000000355 ) ) ;
#6978 = ORIENTED_EDGE ( 'NONE', *, *, #5919, .T. ) ;
#6979 = PRODUCT_CONTEXT ( 'NONE', #7144, 'mechanical' ) ;
#6980 = ORIENTED_EDGE ( 'NONE', *, *, #2473, .F. ) ;
#6981 = DIRECTION ( 'NONE',  ( -0.000000000000000000, 1.000000000000000000, -0.000000000000000000 ) ) ;
#6982 = AXIS2_PLACEMENT_3D ( 'NONE', #10323, #7138, #5378 ) ;
#6983 = ORIENTED_EDGE ( 'NONE', *, *, #142, .F. ) ;
#6984 = ADVANCED_FACE ( 'NONE', ( #368, #1945 ), #5127, .T. ) ;
#6985 = ORIENTED_EDGE ( 'NONE', *, *, #441, .T. ) ;
#6986 = DIRECTION ( 'NONE',  ( 0.000000000000000000, 0.000000000000000000, -1.000000000000000000 ) ) ;
#6987 = FACE_OUTER_BOUND ( 'NONE', #3831, .T. ) ;
#6988 = ORIENTED_EDGE ( 'NONE', *, *, #6186, .F. ) ;
#6989 = SURFACE_STYLE_FILL_AREA ( #1368 ) ;
#6990 = CARTESIAN_POINT ( 'NONE',  ( 39.99999999999997158, -135.1707019118818778, 39.99999999999997868 ) ) ;
#6991 = DIRECTION ( 'NONE',  ( -0.07334937666141773394, 0.9973063064792990762, 0.000000000000000000 ) ) ;
#6992 = VECTOR ( 'NONE', #8178, 1000.000000000000114 ) ;
#6993 = CYLINDRICAL_SURFACE ( 'NONE', #2222, 10.00000000000000178 ) ;
#6994 = CIRCLE ( 'NONE', #4920, 1.999999999999998224 ) ;
#6995 = PLANE ( 'NONE',  #3681 ) ;
#6996 = EDGE_CURVE ( 'NONE', #9384, #735, #5281, .T. ) ;
#6997 = ORIENTED_EDGE ( 'NONE', *, *, #3937, .T. ) ;
#6998 = CARTESIAN_POINT ( 'NONE',  ( -24.15108826162070699, -134.0910007290636941, -50.00000000000001421 ) ) ;
#6999 = AXIS2_PLACEMENT_3D ( 'NONE', #3769, #7004, #2756 ) ;
#7000 = ORIENTED_EDGE ( 'NONE', *, *, #6655, .F. ) ;
#7001 = CARTESIAN_POINT ( 'NONE',  ( -2.293506896408097795, 4.007378841484243628E-15, -28.00000000000002132 ) ) ;
#7002 = FACE_OUTER_BOUND ( 'NONE', #3934, .T. ) ;
#7003 = EDGE_LOOP ( 'NONE', ( #7390, #1900, #5662, #10245 ) ) ;
#7004 = DIRECTION ( 'NONE',  ( -0.000000000000000000, -0.000000000000000000, 1.000000000000000000 ) ) ;
#7005 = DIRECTION ( 'NONE',  ( 0.000000000000000000, 0.000000000000000000, 1.000000000000000000 ) ) ;
#7006 = DIRECTION ( 'NONE',  ( 0.000000000000000000, 1.222897680782651471E-16, 1.000000000000000000 ) ) ;
#7007 = ORIENTED_EDGE ( 'NONE', *, *, #746, .F. ) ;
#7008 = AXIS2_PLACEMENT_3D ( 'NONE', #9054, #3279, #7308 ) ;
#7009 = ORIENTED_EDGE ( 'NONE', *, *, #677, .T. ) ;
#7010 = EDGE_CURVE ( 'NONE', #6356, #6484, #3547, .T. ) ;
#7011 = AXIS2_PLACEMENT_3D ( 'NONE', #9554, #4719, #1381 ) ;
#7012 = ORIENTED_EDGE ( 'NONE', *, *, #2125, .F. ) ;
#7013 = ORIENTED_EDGE ( 'NONE', *, *, #8185, .F. ) ;
#7014 = CARTESIAN_POINT ( 'NONE',  ( -8.793506896408096907, -8.660287962196477451, 0.000000000000000000 ) ) ;
#7015 = CARTESIAN_POINT ( 'NONE',  ( 37.22511195853869026, -115.1457019118818863, 0.000000000000000000 ) ) ;
#7016 = VECTOR ( 'NONE', #6865, 1000.000000000000000 ) ;
#7017 = LINE ( 'NONE', #1235, #10097 ) ;
#7018 = DIRECTION ( 'NONE',  ( 0.000000000000000000, -1.000000000000000000, 1.222897680782651224E-16 ) ) ;
#7019 = CARTESIAN_POINT ( 'NONE',  ( -20.29350689640809691, 140.5696653505793563, -10.90000000000000036 ) ) ;
#7020 = ORIENTED_EDGE ( 'NONE', *, *, #5367, .F. ) ;
#7021 = CARTESIAN_POINT ( 'NONE',  ( 14.70649310359190309, 80.56966535057935630, 24.00000000000000711 ) ) ;
#7022 = EDGE_CURVE ( 'NONE', #8863, #39, #4282, .T. ) ;
#7023 = CIRCLE ( 'NONE', #2777, 5.000000000000000888 ) ;
#7024 = ORIENTED_EDGE ( 'NONE', *, *, #8613, .F. ) ;
#7025 = ORIENTED_EDGE ( 'NONE', *, *, #7734, .T. ) ;
#7026 = DIRECTION ( 'NONE',  ( 0.000000000000000000, 1.000000000000000000, -1.460512169908342690E-16 ) ) ;
#7027 = CARTESIAN_POINT ( 'NONE',  ( -27.15769640663940976, -115.1457019118818863, 25.15769640663938134 ) ) ;
#7028 = CARTESIAN_POINT ( 'NONE',  ( -45.00000000000000000, 0.000000000000000000, 0.000000000000000000 ) ) ;
#7029 = VERTEX_POINT ( 'NONE', #10062 ) ;
#7030 = PLANE ( 'NONE',  #6982 ) ;
#7031 = ADVANCED_FACE ( 'NONE', ( #7516 ), #2848, .T. ) ;
#7032 = EDGE_CURVE ( 'NONE', #8054, #5162, #7726, .T. ) ;
#7033 = EDGE_CURVE ( 'NONE', #6120, #4912, #9004, .T. ) ;
#7034 = ORIENTED_EDGE ( 'NONE', *, *, #2609, .F. ) ;
#7035 = DIRECTION ( 'NONE',  ( 0.000000000000000000, 0.000000000000000000, 1.000000000000000000 ) ) ;
#7036 = VERTEX_POINT ( 'NONE', #2001 ) ;
#7037 = CARTESIAN_POINT ( 'NONE',  ( -30.29350689640809335, 88.56966535057934209, -20.00000000000001066 ) ) ;
#7038 = VERTEX_POINT ( 'NONE', #5232 ) ;
#7039 = ORIENTED_EDGE ( 'NONE', *, *, #6603, .F. ) ;
#7040 = DIRECTION ( 'NONE',  ( 0.000000000000000000, -1.000000000000000000, 1.222897680782651471E-16 ) ) ;
#7041 = CARTESIAN_POINT ( 'NONE',  ( -16.29350689640809691, 65.65569765742554864, 0.000000000000000000 ) ) ;
#7042 = ORIENTED_EDGE ( 'NONE', *, *, #7426, .T. ) ;
#7043 = DIRECTION ( 'NONE',  ( -1.000000000000000000, -0.000000000000000000, -0.000000000000000000 ) ) ;
#7044 = CARTESIAN_POINT ( 'NONE',  ( 0.000000000000000000, -1.467624384280032279, -2.541999999999998039 ) ) ;
#7045 = CARTESIAN_POINT ( 'NONE',  ( 80.08610854271790913, 54.73418909528891874, 30.00000000000000355 ) ) ;
#7046 = CARTESIAN_POINT ( 'NONE',  ( -48.00000000000002132, -117.1457019118819005, 23.15769640663938134 ) ) ;
#7047 = CARTESIAN_POINT ( 'NONE',  ( 3.000000000000000000, 0.000000000000000000, 0.000000000000000000 ) ) ;
#7048 = PRODUCT ( 'Plastic Grip', 'Plastic Grip', '', ( #1520 ) ) ;
#7049 = AXIS2_PLACEMENT_3D ( 'NONE', #7028, #9525, #10262 ) ;
#7050 = ADVANCED_FACE ( 'NONE', ( #8467 ), #1399, .T. ) ;
#7051 = VERTEX_POINT ( 'NONE', #3649 ) ;
#7052 = DIRECTION ( 'NONE',  ( 0.000000000000000000, -0.000000000000000000, 1.000000000000000000 ) ) ;
#7053 = VECTOR ( 'NONE', #1842, 1000.000000000000000 ) ;
#7054 = VERTEX_POINT ( 'NONE', #1844 ) ;
#7055 = CARTESIAN_POINT ( 'NONE',  ( 39.99999999999998579, -135.1707019118818778, -40.00000000000002132 ) ) ;
#7056 = DIRECTION ( 'NONE',  ( 0.000000000000000000, -1.000000000000000000, 0.000000000000000000 ) ) ;
#7057 = AXIS2_PLACEMENT_3D ( 'NONE', #4472, #7602, #5050 ) ;
#7058 = CARTESIAN_POINT ( 'NONE',  ( -2.293506896408097795, 152.5696653505793279, 30.00000000000000355 ) ) ;
#7059 = FACE_OUTER_BOUND ( 'NONE', #4626, .T. ) ;
#7060 = CARTESIAN_POINT ( 'NONE',  ( -147.7878832208476183, 242.6502276555962396, 0.000000000000000000 ) ) ;
#7061 = ORIENTED_EDGE ( 'NONE', *, *, #5993, .T. ) ;
#7062 = AXIS2_PLACEMENT_3D ( 'NONE', #4554, #9436, #7786 ) ;
#7063 = EDGE_LOOP ( 'NONE', ( #3152, #4915, #649, #4839 ) ) ;
#7064 = AXIS2_PLACEMENT_3D ( 'NONE', #579, #1481, #633 ) ;
#7065 = ORIENTED_EDGE ( 'NONE', *, *, #9885, .T. ) ;
#7066 = ORIENTED_EDGE ( 'NONE', *, *, #8828, .F. ) ;
#7067 = CARTESIAN_POINT ( 'NONE',  ( -2.293506896408097795, 0.000000000000000000, 0.000000000000000000 ) ) ;
#7068 = EDGE_CURVE ( 'NONE', #8567, #7162, #881, .T. ) ;
#7069 = DIRECTION ( 'NONE',  ( 0.000000000000000000, -1.000000000000000000, 0.000000000000000000 ) ) ;
#7070 = AXIS2_PLACEMENT_3D ( 'NONE', #6298, #10438, #5502 ) ;
#7071 = LINE ( 'NONE', #3036, #4168 ) ;
#7072 = DIRECTION ( 'NONE',  ( 0.000000000000000000, 0.000000000000000000, 1.000000000000000000 ) ) ;
#7073 = VECTOR ( 'NONE', #9092, 1000.000000000000000 ) ;
#7074 = DIRECTION ( 'NONE',  ( 1.000000000000000000, 0.000000000000000000, 0.000000000000000000 ) ) ;
#7075 = ORIENTED_EDGE ( 'NONE', *, *, #8077, .F. ) ;
#7076 = CARTESIAN_POINT ( 'NONE',  ( -16.29350689640809691, 105.5289575273812233, 10.90000000000000036 ) ) ;
#7077 = AXIS2_PLACEMENT_3D ( 'NONE', #5582, #2252, #5477 ) ;
#7078 = VERTEX_POINT ( 'NONE', #7673 ) ;
#7079 = VECTOR ( 'NONE', #5566, 1000.000000000000000 ) ;
#7080 = CARTESIAN_POINT ( 'NONE',  ( -159.0987744993230706, 269.0617377047655054, 4.136592538792403018E-16 ) ) ;
#7081 = EDGE_CURVE ( 'NONE', #9607, #1028, #9011, .T. ) ;
#7082 = VECTOR ( 'NONE', #3676, 1000.000000000000000 ) ;
#7083 =( REPRESENTATION_RELATIONSHIP ('NONE','NONE', #9007, #5068 ) REPRESENTATION_RELATIONSHIP_WITH_TRANSFORMATION ( #7240 )SHAPE_REPRESENTATION_RELATIONSHIP( ) );
#7084 = CARTESIAN_POINT ( 'NONE',  ( -39.94539818030332157, 129.0132282531173757, -3.999999999999991562 ) ) ;
#7085 = DIRECTION ( 'NONE',  ( 1.000000000000000000, 0.000000000000000000, 0.000000000000000000 ) ) ;
#7086 = DIRECTION ( 'NONE',  ( -1.000000000000000000, 0.000000000000000000, 0.000000000000000000 ) ) ;
#7087 = VERTEX_POINT ( 'NONE', #3487 ) ;
#7088 = DIRECTION ( 'NONE',  ( 0.000000000000000000, 1.000000000000000000, 0.000000000000000000 ) ) ;
#7089 = VERTEX_POINT ( 'NONE', #5971 ) ;
#7090 = AXIS2_PLACEMENT_3D ( 'NONE', #9385, #10181, #5294 ) ;
#7091 = DIRECTION ( 'NONE',  ( -0.6691306063588553510, -0.7431448254773969087, 0.000000000000000000 ) ) ;
#7092 = EDGE_LOOP ( 'NONE', ( #60, #4459 ) ) ;
#7093 = EDGE_LOOP ( 'NONE', ( #6286, #8253, #6964, #2584 ) ) ;
#7094 = CARTESIAN_POINT ( 'NONE',  ( 3.000000000000000000, 2.935248768560057897, -3.252606517456513302E-15 ) ) ;
#7095 = ADVANCED_FACE ( 'NONE', ( #8361 ), #8158, .F. ) ;
#7096 = DIRECTION ( 'NONE',  ( -0.000000000000000000, -1.000000000000000000, -0.000000000000000000 ) ) ;
#7097 = EDGE_CURVE ( 'NONE', #9778, #732, #8835, .T. ) ;
#7098 = EDGE_CURVE ( 'NONE', #9534, #86, #8669, .T. ) ;
#7099 = FACE_OUTER_BOUND ( 'NONE', #2393, .T. ) ;
#7100 = DIRECTION ( 'NONE',  ( 0.000000000000000000, 0.000000000000000000, 1.000000000000000000 ) ) ;
#7101 = CARTESIAN_POINT ( 'NONE',  ( -166.0794662972351716, 270.8019239353934040, 0.000000000000000000 ) ) ;
#7102 = DIRECTION ( 'NONE',  ( 0.000000000000000000, -0.000000000000000000, 1.000000000000000000 ) ) ;
#7103 = LINE ( 'NONE', #10336, #2336 ) ;
#7104 = AXIS2_PLACEMENT_3D ( 'NONE', #1928, #10045, #8399 ) ;
#7105 = VERTEX_POINT ( 'NONE', #9213 ) ;
#7106 = DIRECTION ( 'NONE',  ( -1.000000000000000000, 0.000000000000000000, 0.000000000000000000 ) ) ;
#7107 = ORIENTED_EDGE ( 'NONE', *, *, #10280, .F. ) ;
#7108 = PRODUCT_RELATED_PRODUCT_CATEGORY ( 'part', '', ( #5424 ) ) ;
#7109 = CARTESIAN_POINT ( 'NONE',  ( -20.29350689640809691, 140.5696653505793563, 7.750000000000001776 ) ) ;
#7110 = FILL_AREA_STYLE_COLOUR ( '', #2395 ) ;
#7111 = EDGE_CURVE ( 'NONE', #2586, #6030, #2268, .T. ) ;
#7112 = ADVANCED_FACE ( 'NONE', ( #7281 ), #9424, .T. ) ;
#7113 = VERTEX_POINT ( 'NONE', #10331 ) ;
#7114 = AXIS2_PLACEMENT_3D ( 'NONE', #4356, #7592, #4249 ) ;
#7115 = FACE_OUTER_BOUND ( 'NONE', #697, .T. ) ;
#7116 = DIRECTION ( 'NONE',  ( 0.000000000000000000, 0.000000000000000000, 1.000000000000000000 ) ) ;
#7117 = DIRECTION ( 'NONE',  ( -1.000000000000000000, 0.000000000000000000, -0.000000000000000000 ) ) ;
#7118 = EDGE_LOOP ( 'NONE', ( #1257, #4005, #6876, #69 ) ) ;
#7119 = ORIENTED_EDGE ( 'NONE', *, *, #8315, .F. ) ;
#7120 = VERTEX_POINT ( 'NONE', #1313 ) ;
#7121 = EDGE_LOOP ( 'NONE', ( #1411, #5476, #1139 ) ) ;
#7122 = LINE ( 'NONE', #2187, #2337 ) ;
#7123 = CARTESIAN_POINT ( 'NONE',  ( 37.22511195853866894, 17.84145331825995839, -24.99999999999998934 ) ) ;
#7124 = PLANE ( 'NONE',  #8571 ) ;
#7125 = CARTESIAN_POINT ( 'NONE',  ( -39.94539818030332157, 145.0132282531173189, -3.999999999999988898 ) ) ;
#7126 = DIRECTION ( 'NONE',  ( 0.000000000000000000, -0.000000000000000000, -1.000000000000000000 ) ) ;
#7127 = ORIENTED_EDGE ( 'NONE', *, *, #3867, .T. ) ;
#7128 = DIRECTION ( 'NONE',  ( 0.000000000000000000, 0.000000000000000000, -1.000000000000000000 ) ) ;
#7129 = EDGE_CURVE ( 'NONE', #1889, #10187, #3422, .T. ) ;
#7130 = VERTEX_POINT ( 'NONE', #4052 ) ;
#7131 = DIRECTION ( 'NONE',  ( 0.000000000000000000, 0.000000000000000000, -1.000000000000000000 ) ) ;
#7132 = PRODUCT_DEFINITION_SHAPE ( 'NONE', 'NONE',  #10480 ) ;
#7133 = LINE ( 'NONE', #4088, #4688 ) ;
#7134 = LINE ( 'NONE', #9524, #1769 ) ;
#7135 = CARTESIAN_POINT ( 'NONE',  ( -48.00000000000002132, -117.1457019118819005, -23.15769640663945594 ) ) ;
#7136 = EDGE_LOOP ( 'NONE', ( #8784, #4904, #927, #6675 ) ) ;
#7137 = AXIS2_PLACEMENT_3D ( 'NONE', #729, #8628, #9595 ) ;
#7138 = DIRECTION ( 'NONE',  ( 0.000000000000000000, -1.000000000000000000, -0.000000000000000000 ) ) ;
#7139 = APPLICATION_PROTOCOL_DEFINITION ( 'draft international standard', 'automotive_design', 1998, #7144 ) ;
#7140 = VERTEX_POINT ( 'NONE', #1420 ) ;
#7141 = CARTESIAN_POINT ( 'NONE',  ( 26.00000000000000355, 3.334407072378455680E-16, -2.445500000000000007 ) ) ;
#7142 = ORIENTED_EDGE ( 'NONE', *, *, #5499, .F. ) ;
#7143 = CIRCLE ( 'NONE', #6624, 4.000000000000003553 ) ;
#7144 = APPLICATION_CONTEXT ( 'automotive_design' ) ;
#7145 = EDGE_LOOP ( 'NONE', ( #5704, #8593, #4483, #5615 ) ) ;
#7146 = LINE ( 'NONE', #7094, #2133 ) ;
#7147 = SURFACE_STYLE_USAGE ( .BOTH. , #3915 ) ;
#7148 = CARTESIAN_POINT ( 'NONE',  ( -47.94539818030330025, 150.5696653505793563, 4.025000000000000355 ) ) ;
#7149 = FACE_OUTER_BOUND ( 'NONE', #4660, .T. ) ;
#7150 = FACE_OUTER_BOUND ( 'NONE', #1985, .T. ) ;
#7151 = DIRECTION ( 'NONE',  ( 0.000000000000000000, 0.000000000000000000, 1.000000000000000000 ) ) ;
#7152 = AXIS2_PLACEMENT_3D ( 'NONE', #4834, #815, #2104 ) ;
#7153 = EDGE_CURVE ( 'NONE', #3513, #7537, #7316, .T. ) ;
#7154 = ORIENTED_EDGE ( 'NONE', *, *, #2449, .T. ) ;
#7155 = CARTESIAN_POINT ( 'NONE',  ( -25.15769640663939199, -133.1457019118818721, -27.15769640663944173 ) ) ;
#7156 = ORIENTED_EDGE ( 'NONE', *, *, #5725, .F. ) ;
#7157 = DIRECTION ( 'NONE',  ( 0.000000000000000000, 0.000000000000000000, 1.000000000000000000 ) ) ;
#7158 =( LENGTH_UNIT ( ) NAMED_UNIT ( * ) SI_UNIT ( .MILLI., .METRE. ) );
#7159 = DIRECTION ( 'NONE',  ( -0.000000000000000000, -1.000000000000000000, -0.000000000000000000 ) ) ;
#7160 = CARTESIAN_POINT ( 'NONE',  ( -31.74999999999995737, 0.000000000000000000, 5.000000000000000000 ) ) ;
#7161 = DIRECTION ( 'NONE',  ( 1.000000000000000000, 0.000000000000000000, 0.000000000000000000 ) ) ;
#7162 = VERTEX_POINT ( 'NONE', #3863 ) ;
#7163 = ORIENTED_EDGE ( 'NONE', *, *, #894, .T. ) ;
#7164 = ADVANCED_FACE ( 'NONE', ( #22 ), #2454, .F. ) ;
#7165 = EDGE_CURVE ( 'NONE', #9778, #6079, #5680, .T. ) ;
#7166 = CIRCLE ( 'NONE', #8004, 2.525240063345735475 ) ;
#7167 = ADVANCED_FACE ( 'NONE', ( #2954 ), #5953, .F. ) ;
#7168 = ORIENTED_EDGE ( 'NONE', *, *, #5980, .T. ) ;
#7169 = CARTESIAN_POINT ( 'NONE',  ( -16.29350689640809691, -186.9457019118818835, 7.500000000000000000 ) ) ;
#7170 = DIRECTION ( 'NONE',  ( -1.000000000000000000, -0.000000000000000000, 0.000000000000000000 ) ) ;
#7171 = VERTEX_POINT ( 'NONE', #1665 ) ;
#7172 = CARTESIAN_POINT ( 'NONE',  ( -7.293506896408097795, 145.5696653505793563, 25.00000000000000711 ) ) ;
#7173 = DIRECTION ( 'NONE',  ( 0.000000000000000000, 1.000000000000000000, 0.000000000000000000 ) ) ;
#7174 = CIRCLE ( 'NONE', #2419, 5.000000000000000888 ) ;
#7175 = DIRECTION ( 'NONE',  ( 0.000000000000000000, -1.000000000000000000, 0.000000000000000000 ) ) ;
#7176 = ORIENTED_EDGE ( 'NONE', *, *, #1574, .F. ) ;
#7177 = FACE_OUTER_BOUND ( 'NONE', #7378, .T. ) ;
#7178 = EDGE_CURVE ( 'NONE', #5603, #9316, #3248, .T. ) ;
#7179 = AXIS2_PLACEMENT_3D ( 'NONE', #6828, #6722, #4442 ) ;
#7180 = ORIENTED_EDGE ( 'NONE', *, *, #3125, .T. ) ;
#7181 = CARTESIAN_POINT ( 'NONE',  ( -16.29350689640809691, -115.1457019118818863, -30.31717237747080773 ) ) ;
#7182 = PRODUCT_DEFINITION_FORMATION_WITH_SPECIFIED_SOURCE ( 'ANY', '', #5681, .NOT_KNOWN. ) ;
#7183 = FACE_OUTER_BOUND ( 'NONE', #2991, .T. ) ;
#7184 = DIRECTION ( 'NONE',  ( 0.000000000000000000, 1.224646799147351482E-16, 1.000000000000000000 ) ) ;
#7185 = AXIS2_PLACEMENT_3D ( 'NONE', #7505, #8404, #7558 ) ;
#7186 = ORIENTED_EDGE ( 'NONE', *, *, #6644, .F. ) ;
#7187 = FACE_OUTER_BOUND ( 'NONE', #10350, .T. ) ;
#7188 = CARTESIAN_POINT ( 'NONE',  ( -30.29350689640809335, 120.5696653505793705, 24.00000000000000711 ) ) ;
#7189 = ORIENTED_EDGE ( 'NONE', *, *, #357, .T. ) ;
#7190 = CARTESIAN_POINT ( 'NONE',  ( -2.293506896408094242, 37.08684478514405214, -12.50000000000000000 ) ) ;
#7191 = VERTEX_POINT ( 'NONE', #9728 ) ;
#7192 = AXIS2_PLACEMENT_3D ( 'NONE', #5682, #8235, #8125 ) ;
#7193 = ORIENTED_EDGE ( 'NONE', *, *, #8790, .T. ) ;
#7194 = LINE ( 'NONE', #9478, #1623 ) ;
#7195 = EDGE_CURVE ( 'NONE', #8587, #2261, #3751, .T. ) ;
#7196 = DIRECTION ( 'NONE',  ( -1.000000000000000000, 0.000000000000000000, 0.000000000000000000 ) ) ;
#7197 = AXIS2_PLACEMENT_3D ( 'NONE', #2433, #9866, #107 ) ;
#7198 = DIRECTION ( 'NONE',  ( -1.000000000000000000, 0.000000000000000000, 0.000000000000000000 ) ) ;
#7199 = DIRECTION ( 'NONE',  ( -0.000000000000000000, -1.000000000000000000, -0.000000000000000000 ) ) ;
#7200 = FACE_OUTER_BOUND ( 'NONE', #7121, .T. ) ;
#7201 = DIRECTION ( 'NONE',  ( 0.000000000000000000, 1.000000000000000000, 1.224646799147353207E-16 ) ) ;
#7202 = ORIENTED_EDGE ( 'NONE', *, *, #155, .F. ) ;
#7203 = DIRECTION ( 'NONE',  ( -6.982941293900105430E-16, 0.000000000000000000, 1.000000000000000000 ) ) ;
#7204 = ORIENTED_EDGE ( 'NONE', *, *, #3761, .T. ) ;
#7205 = CYLINDRICAL_SURFACE ( 'NONE', #8943, 2.000000000000001776 ) ;
#7206 = DIRECTION ( 'NONE',  ( 0.000000000000000000, 0.000000000000000000, 1.000000000000000000 ) ) ;
#7207 = DIRECTION ( 'NONE',  ( 1.000000000000000000, 3.081165567444019513E-16, -0.000000000000000000 ) ) ;
#7208 = EDGE_CURVE ( 'NONE', #4536, #6699, #8675, .T. ) ;
#7209 = DIRECTION ( 'NONE',  ( 0.000000000000000000, 0.000000000000000000, 1.000000000000000000 ) ) ;
#7210 = AXIS2_PLACEMENT_3D ( 'NONE', #2311, #8718, #2939 ) ;
#7211 = FACE_OUTER_BOUND ( 'NONE', #6430, .T. ) ;
#7212 = ORIENTED_EDGE ( 'NONE', *, *, #6835, .T. ) ;
#7213 = ORIENTED_EDGE ( 'NONE', *, *, #2219, .F. ) ;
#7214 = AXIS2_PLACEMENT_3D ( 'NONE', #2210, #572, #624 ) ;
#7215 = CIRCLE ( 'NONE', #7387, 7.525240063345735031 ) ;
#7216 = EDGE_LOOP ( 'NONE', ( #7034, #2965, #3861, #306 ) ) ;
#7217 = CARTESIAN_POINT ( 'NONE',  ( -7.293506896408097795, 80.56966535057935630, 28.00000000000001066 ) ) ;
#7218 = CARTESIAN_POINT ( 'NONE',  ( -39.65624476065124782, -3.117691453623975484, -1.800000000000017586 ) ) ;
#7219 = CARTESIAN_POINT ( 'NONE',  ( -20.14472382240651882, -141.8229441850657793, -25.87097612368021160 ) ) ;
#7220 = CARTESIAN_POINT ( 'NONE',  ( 0.000000000000000000, 55.56966535057937051, 10.98204862120179826 ) ) ;
#7221 = ADVANCED_FACE ( 'NONE', ( #6987 ), #7885, .F. ) ;
#7222 = EDGE_CURVE ( 'NONE', #852, #10322, #2158, .T. ) ;
#7223 = EDGE_CURVE ( 'NONE', #1967, #9556, #79, .T. ) ;
#7224 = CARTESIAN_POINT ( 'NONE',  ( -27.15769640663937778, -135.1457019118818721, -48.00000000000002132 ) ) ;
#7225 = CIRCLE ( 'NONE', #2325, 5.000000000000000000 ) ;
#7226 = VERTEX_POINT ( 'NONE', #519 ) ;
#7227 = FACE_OUTER_BOUND ( 'NONE', #442, .T. ) ;
#7228 = VECTOR ( 'NONE', #6875, 1000.000000000000000 ) ;
#7229 = ORIENTED_EDGE ( 'NONE', *, *, #3597, .T. ) ;
#7230 = DIRECTION ( 'NONE',  ( -8.194486552889013533E-17, -9.100899318238110877E-17, 1.000000000000000000 ) ) ;
#7231 = AXIS2_PLACEMENT_3D ( 'NONE', #8086, #8246, #4063 ) ;
#7232 = ADVANCED_FACE ( 'NONE', ( #6182 ), #1366, .T. ) ;
#7233 = EDGE_CURVE ( 'NONE', #719, #5823, #4267, .T. ) ;
#7234 = DIRECTION ( 'NONE',  ( -1.000000000000000000, 0.000000000000000000, 0.000000000000000000 ) ) ;
#7235 = FACE_OUTER_BOUND ( 'NONE', #4740, .T. ) ;
#7236 = CLOSED_SHELL ( 'NONE', ( #1745, #7616, #2779, #7167, #3011, #5584, #4590, #8245, #4881, #6702, #7607, #9277, #1259, #5802, #7918, #9095, #6247, #238, #9111, #2080, #7410, #6837, #3461, #2993, #8538 ) ) ;
#7237 = ORIENTED_EDGE ( 'NONE', *, *, #7301, .F. ) ;
#7238 = CARTESIAN_POINT ( 'NONE',  ( -16.29350689640809691, 88.12362273389504708, 0.000000000000000000 ) ) ;
#7239 = AXIS2_PLACEMENT_3D ( 'NONE', #4922, #3397, #8277 ) ;
#7240 = ITEM_DEFINED_TRANSFORMATION ( 'NONE', 'NONE', #9727,  #4601 ) ;
#7241 = ORIENTED_EDGE ( 'NONE', *, *, #1490, .T. ) ;
#7242 = DIRECTION ( 'NONE',  ( 1.000000000000000000, 0.000000000000000000, 0.000000000000000000 ) ) ;
#7243 = ORIENTED_EDGE ( 'NONE', *, *, #2414, .F. ) ;
#7244 = VECTOR ( 'NONE', #3984, 1000.000000000000000 ) ;
#7245 = EDGE_LOOP ( 'NONE', ( #407, #8154, #807, #8615 ) ) ;
#7246 = CARTESIAN_POINT ( 'NONE',  ( 14.70649310359190309, 80.56966535057935630, -24.00000000000000711 ) ) ;
#7247 = CARTESIAN_POINT ( 'NONE',  ( 4.856471286862175774, 152.5696653505793279, -25.00000000000001776 ) ) ;
#7248 = FACE_OUTER_BOUND ( 'NONE', #1788, .T. ) ;
#7249 = DIRECTION ( 'NONE',  ( 1.000000000000000000, 0.000000000000000000, 0.000000000000000000 ) ) ;
#7250 = DIRECTION ( 'NONE',  ( -0.000000000000000000, -0.000000000000000000, 1.000000000000000000 ) ) ;
#7251 = VECTOR ( 'NONE', #9052, 1000.000000000000000 ) ;
#7252 = ADVANCED_FACE ( 'NONE', ( #2714 ), #1075, .T. ) ;
#7253 = ORIENTED_EDGE ( 'NONE', *, *, #3167, .F. ) ;
#7254 = CARTESIAN_POINT ( 'NONE',  ( -27.15769640663939555, -135.1457019118818721, -25.15769640663944173 ) ) ;
#7255 = ORIENTED_EDGE ( 'NONE', *, *, #5371, .F. ) ;
#7256 = EDGE_CURVE ( 'NONE', #7422, #7140, #5153, .T. ) ;
#7257 = CARTESIAN_POINT ( 'NONE',  ( -30.29350689640809335, 120.5696653505793705, 16.00000000000000711 ) ) ;
#7258 = CARTESIAN_POINT ( 'NONE',  ( -30.29350689640809335, 120.5696653505793705, -27.99999999999999645 ) ) ;
#7259 = VECTOR ( 'NONE', #6611, 1000.000000000000000 ) ;
#7260 = CARTESIAN_POINT ( 'NONE',  ( -23.76520584195948516, -145.1457019118819005, -97.78965767959371647 ) ) ;
#7261 = FACE_OUTER_BOUND ( 'NONE', #5330, .T. ) ;
#7262 = DIRECTION ( 'NONE',  ( -0.000000000000000000, 1.000000000000000000, -0.000000000000000000 ) ) ;
#7263 = DIRECTION ( 'NONE',  ( -0.000000000000000000, -1.000000000000000000, -0.000000000000000000 ) ) ;
#7264 = VECTOR ( 'NONE', #4827, 1000.000000000000000 ) ;
#7265 = EDGE_LOOP ( 'NONE', ( #4236, #5623, #5434, #4982, #6527 ) ) ;
#7266 = ORIENTED_EDGE ( 'NONE', *, *, #2091, .F. ) ;
#7267 = EDGE_CURVE ( 'NONE', #640, #2261, #9178, .T. ) ;
#7268 = EDGE_LOOP ( 'NONE', ( #2232, #4091, #5149 ) ) ;
#7269 = COLOUR_RGB ( '',0.7921568627450980005, 0.8196078431372548767, 0.9333333333333333481 ) ;
#7270 = DIRECTION ( 'NONE',  ( -1.000000000000000000, 0.000000000000000000, 0.000000000000000000 ) ) ;
#7271 = DIRECTION ( 'NONE',  ( 0.000000000000000000, 0.000000000000000000, -1.000000000000000000 ) ) ;
#7272 = CARTESIAN_POINT ( 'NONE',  ( -47.94539818030330025, 137.0132282531173473, -3.999999999999991562 ) ) ;
#7273 = VERTEX_POINT ( 'NONE', #9029 ) ;
#7274 = LINE ( 'NONE', #5775, #1479 ) ;
#7275 = ORIENTED_EDGE ( 'NONE', *, *, #6432, .T. ) ;
#7276 = DIRECTION ( 'NONE',  ( -0.7431448254773957984, 0.6691306063588565722, -0.000000000000000000 ) ) ;
#7277 = ADVANCED_FACE ( 'NONE', ( #294 ), #7386, .F. ) ;
#7278 = EDGE_CURVE ( 'NONE', #2007, #4617, #9945, .T. ) ;
#7279 = VERTEX_POINT ( 'NONE', #7601 ) ;
#7280 = FACE_OUTER_BOUND ( 'NONE', #7093, .T. ) ;
#7281 = FACE_OUTER_BOUND ( 'NONE', #9671, .T. ) ;
#7282 = DIRECTION ( 'NONE',  ( 1.000000000000000000, 0.000000000000000000, 0.000000000000000000 ) ) ;
#7283 = CARTESIAN_POINT ( 'NONE',  ( -40.00000000000001421, -135.1457019118818721, -35.97500000000002274 ) ) ;
#7284 = ORIENTED_EDGE ( 'NONE', *, *, #10280, .T. ) ;
#7285 = CARTESIAN_POINT ( 'NONE',  ( -16.29350689640809691, -186.9457019118818835, 27.01918567566963247 ) ) ;
#7286 = ITEM_DEFINED_TRANSFORMATION ( 'NONE', 'NONE', #9038,  #4601 ) ;
#7287 = ADVANCED_FACE ( 'NONE', ( #5942 ), #8977, .T. ) ;
#7289 = EDGE_CURVE ( 'NONE', #6699, #2391, #4766, .T. ) ;
#7288 = ORIENTED_EDGE ( 'NONE', *, *, #5859, .T. ) ;
#7290 = EDGE_CURVE ( 'NONE', #996, #4419, #2667, .T. ) ;
#7291 = LINE ( 'NONE', #9736, #2345 ) ;
#7292 = ORIENTED_EDGE ( 'NONE', *, *, #618, .F. ) ;
#7293 = LINE ( 'NONE', #6604, #8583 ) ;
#7294 = AXIS2_PLACEMENT_3D ( 'NONE', #6292, #2369, #7249 ) ;
#7295 = CARTESIAN_POINT ( 'NONE',  ( -23.76520584195948516, -145.1457019118819005, -0.6509338422960262438 ) ) ;
#7296 = DIRECTION ( 'NONE',  ( -0.000000000000000000, -0.000000000000000000, 1.000000000000000000 ) ) ;
#7297 = CARTESIAN_POINT ( 'NONE',  ( -23.15769640663940976, -115.1457019118818863, 47.99999999999997868 ) ) ;
#7298 = CARTESIAN_POINT ( 'NONE',  ( -16.29350689640809691, -8.660287962196477451, 0.000000000000000000 ) ) ;
#7299 = ORIENTED_EDGE ( 'NONE', *, *, #3761, .F. ) ;
#7300 = VECTOR ( 'NONE', #1671, 1000.000000000000000 ) ;
#7301 = EDGE_CURVE ( 'NONE', #6648, #9925, #7486, .T. ) ;
#7302 = CARTESIAN_POINT ( 'NONE',  ( -21.29350689640810046, 105.5289575273812233, 7.750000000000000888 ) ) ;
#7303 = VECTOR ( 'NONE', #78, 1000.000000000000000 ) ;
#7304 = VERTEX_POINT ( 'NONE', #5790 ) ;
#7305 = DIRECTION ( 'NONE',  ( 1.137729606058012035E-16, 0.000000000000000000, 1.000000000000000000 ) ) ;
#7306 = FACE_OUTER_BOUND ( 'NONE', #410, .T. ) ;
#7307 =( NAMED_UNIT ( * ) PLANE_ANGLE_UNIT ( ) SI_UNIT ( $, .RADIAN. ) );
#7308 = DIRECTION ( 'NONE',  ( -0.6691306063588565722, -0.7431448254773959095, 0.000000000000000000 ) ) ;
#7309 = EDGE_CURVE ( 'NONE', #2474, #9955, #2400, .T. ) ;
#7310 = CARTESIAN_POINT ( 'NONE',  ( 23.15769640663936713, -115.1457019118818863, 49.99999999999997868 ) ) ;
#7311 = AXIS2_PLACEMENT_3D ( 'NONE', #3222, #4961, #5814 ) ;
#7312 = CARTESIAN_POINT ( 'NONE',  ( -129.7734861572812974, 221.9362163441986411, 0.000000000000000000 ) ) ;
#7313 = EDGE_LOOP ( 'NONE', ( #5625, #5676, #797, #9683 ) ) ;
#7314 = ORIENTED_EDGE ( 'NONE', *, *, #2233, .F. ) ;
#7315 = ORIENTED_EDGE ( 'NONE', *, *, #8775, .F. ) ;
#7316 = CIRCLE ( 'NONE', #3935, 1.999999999999998224 ) ;
#7317 = ORIENTED_EDGE ( 'NONE', *, *, #8765, .F. ) ;
#7318 = VECTOR ( 'NONE', #2093, 1000.000000000000000 ) ;
#7319 = LINE ( 'NONE', #63, #9450 ) ;
#7320 = DIRECTION ( 'NONE',  ( 0.000000000000000000, 0.000000000000000000, -1.000000000000000000 ) ) ;
#7321 = LINE ( 'NONE', #2495, #8685 ) ;
#7322 = EDGE_CURVE ( 'NONE', #9202, #6927, #3767, .T. ) ;
#7323 = CARTESIAN_POINT ( 'NONE',  ( -24.31850689640809549, 140.5696653505793563, 20.00000000000002132 ) ) ;
#7324 = ORIENTED_EDGE ( 'NONE', *, *, #9537, .F. ) ;
#7325 = B_SPLINE_CURVE_WITH_KNOTS ( 'NONE', 3,
 ( #10238, #1171, #2970, #6200, #9443, #5138, #3559, #6782, #4349, #4404 ),
 .UNSPECIFIED., .F., .F.,
 ( 4, 2, 2, 2, 4 ),
 ( 0.000000000000000000, 0.001023740819106953685, 0.002047481638213907371, 0.003071222457320861056, 0.004094963276427814741 ),
 .UNSPECIFIED. ) ;
#7326 = DIRECTION ( 'NONE',  ( 0.9973063064792990762, 0.07334937666141773394, 0.000000000000000000 ) ) ;
#7327 = EDGE_CURVE ( 'NONE', #3326, #7029, #5114, .T. ) ;
#7328 = ORIENTED_EDGE ( 'NONE', *, *, #2449, .F. ) ;
#7329 = VECTOR ( 'NONE', #398, 1000.000000000000000 ) ;
#7330 =( LENGTH_UNIT ( ) NAMED_UNIT ( * ) SI_UNIT ( .MILLI., .METRE. ) );
#7331 = ORIENTED_EDGE ( 'NONE', *, *, #690, .F. ) ;
#7332 = CARTESIAN_POINT ( 'NONE',  ( 3.000000000000000000, 1.467624384280032501, 2.541999999999999371 ) ) ;
#7333 = CARTESIAN_POINT ( 'NONE',  ( -50.00000000000002132, -133.1457019118818721, -23.15769640663945594 ) ) ;
#7334 = DIRECTION ( 'NONE',  ( 0.000000000000000000, 0.4226182617407067132, -0.9063077870366466060 ) ) ;
#7335 = DIRECTION ( 'NONE',  ( -0.000000000000000000, 0.000000000000000000, 1.000000000000000000 ) ) ;
#7336 = EDGE_CURVE ( 'NONE', #9783, #6462, #3465, .T. ) ;
#7337 = DIRECTION ( 'NONE',  ( 0.000000000000000000, 0.000000000000000000, 1.000000000000000000 ) ) ;
#7338 = ORIENTED_EDGE ( 'NONE', *, *, #6900, .T. ) ;
#7339 = CARTESIAN_POINT ( 'NONE',  ( -23.15769640663939199, -117.1457019118819005, -27.15769640663944173 ) ) ;
#7340 = CIRCLE ( 'NONE', #1919, 2.525240063345735475 ) ;
#7341 = EDGE_LOOP ( 'NONE', ( #2598, #9072, #966, #1838, #1804 ) ) ;
#7342 = CARTESIAN_POINT ( 'NONE',  ( -24.98777100551300023, -134.6884840344297913, 49.99999999999998579 ) ) ;
#7343 = ORIENTED_EDGE ( 'NONE', *, *, #3149, .T. ) ;
#7344 = VERTEX_POINT ( 'NONE', #4257 ) ;
#7345 = AXIS2_PLACEMENT_3D ( 'NONE', #4596, #1573, #7198 ) ;
#7346 = CARTESIAN_POINT ( 'NONE',  ( -23.48622939173158386, -144.8896666241527669, -3.853145670227909658 ) ) ;
#7347 = EDGE_CURVE ( 'NONE', #9534, #1811, #4208, .T. ) ;
#7348 = EDGE_CURVE ( 'NONE', #3068, #8465, #8233, .T. ) ;
#7349 = CYLINDRICAL_SURFACE ( 'NONE', #6863, 3.999999999999998668 ) ;
#7350 = PRODUCT_DEFINITION_FORMATION_WITH_SPECIFIED_SOURCE ( 'ANY', '', #9406, .NOT_KNOWN. ) ;
#7351 = EDGE_CURVE ( 'NONE', #7113, #8587, #6643, .T. ) ;
#7352 = SPHERICAL_SURFACE ( 'NONE', #5259, 2.000000000000000000 ) ;
#7353 = CARTESIAN_POINT ( 'NONE',  ( -7.293506896408097795, 0.000000000000000000, 0.000000000000000000 ) ) ;
#7354 = ORIENTED_EDGE ( 'NONE', *, *, #833, .T. ) ;
#7355 = CIRCLE ( 'NONE', #7192, 24.24539146688411861 ) ;
#7356 = LINE ( 'NONE', #205, #6717 ) ;
#7357 = VERTEX_POINT ( 'NONE', #9994 ) ;
#7358 = DIRECTION ( 'NONE',  ( 1.000000000000000000, 0.000000000000000000, 0.000000000000000000 ) ) ;
#7359 = CARTESIAN_POINT ( 'NONE',  ( 0.000000000000000000, 0.000000000000000000, -10.90000000000000036 ) ) ;
#7360 = CARTESIAN_POINT ( 'NONE',  ( 42.22511195853868315, -135.1457019118818721, 25.00000000000000000 ) ) ;
#7361 = DIRECTION ( 'NONE',  ( -0.000000000000000000, 1.000000000000000000, -0.000000000000000000 ) ) ;
#7362 = CARTESIAN_POINT ( 'NONE',  ( -16.29350689640809691, 105.5289575273812233, 10.90000000000000036 ) ) ;
#7363 = VECTOR ( 'NONE', #842, 1000.000000000000114 ) ;
#7364 = EDGE_CURVE ( 'NONE', #4025, #5863, #2921, .T. ) ;
#7365 = DIRECTION ( 'NONE',  ( 3.081165567444019513E-16, -1.000000000000000000, 0.000000000000000000 ) ) ;
#7366 = ORIENTED_EDGE ( 'NONE', *, *, #995, .T. ) ;
#7367 = ORIENTED_EDGE ( 'NONE', *, *, #7542, .T. ) ;
#7368 = ORIENTED_EDGE ( 'NONE', *, *, #3849, .T. ) ;
#7369 = EDGE_LOOP ( 'NONE', ( #6571, #6633, #5515, #6800 ) ) ;
#7370 = CARTESIAN_POINT ( 'NONE',  ( -39.00428932080996702, -3.065011249696382389, -1.804608920635915492 ) ) ;
#7371 = AXIS2_PLACEMENT_3D ( 'NONE', #2272, #4705, #5552 ) ;
#7372 = EDGE_LOOP ( 'NONE', ( #5844, #9698, #2770, #4792 ) ) ;
#7373 = CARTESIAN_POINT ( 'NONE',  ( 37.59878849545336976, 37.08684478514406635, 12.50000000000000711 ) ) ;
#7374 = DIRECTION ( 'NONE',  ( 1.000000000000000000, 0.000000000000000000, 0.000000000000000000 ) ) ;
#7375 = ORIENTED_EDGE ( 'NONE', *, *, #3194, .F. ) ;
#7376 = DIRECTION ( 'NONE',  ( 9.101836848464095537E-17, 0.000000000000000000, 1.000000000000000000 ) ) ;
#7377 = AXIS2_PLACEMENT_3D ( 'NONE', #5126, #8360, #469 ) ;
#7378 = EDGE_LOOP ( 'NONE', ( #2557, #8291, #7923, #3129 ) ) ;
#7379 = EDGE_CURVE ( 'NONE', #1443, #4078, #5121, .T. ) ;
#7380 = ORIENTED_EDGE ( 'NONE', *, *, #6310, .T. ) ;
#7381 = UNCERTAINTY_MEASURE_WITH_UNIT (LENGTH_MEASURE( 1.000000000000000082E-05 ), #5955, 'distance_accuracy_value', 'NONE');
#7382 = CARTESIAN_POINT ( 'NONE',  ( -2.293506896408097795, 37.08684478514406635, 30.00000000000000355 ) ) ;
#7383 = DIRECTION ( 'NONE',  ( 0.000000000000000000, -1.000000000000000000, 0.000000000000000000 ) ) ;
#7384 = AXIS2_PLACEMENT_3D ( 'NONE', #2277, #6502, #2423 ) ;
#7385 = DIRECTION ( 'NONE',  ( -1.000000000000000000, -0.000000000000000000, -0.000000000000000000 ) ) ;
#7386 = PLANE ( 'NONE',  #2063 ) ;
#7387 = AXIS2_PLACEMENT_3D ( 'NONE', #4785, #9841, #3306 ) ;
#7388 = CARTESIAN_POINT ( 'NONE',  ( -16.26850689640809833, 140.5696653505793563, 10.90000000000000036 ) ) ;
#7389 = DIRECTION ( 'NONE',  ( 0.000000000000000000, 0.000000000000000000, 1.000000000000000000 ) ) ;
#7390 = ORIENTED_EDGE ( 'NONE', *, *, #3538, .F. ) ;
#7391 = FACE_OUTER_BOUND ( 'NONE', #8654, .T. ) ;
#7392 = AXIS2_PLACEMENT_3D ( 'NONE', #7722, #1362, #1254 ) ;
#7393 = ORIENTED_EDGE ( 'NONE', *, *, #5725, .T. ) ;
#7394 = VECTOR ( 'NONE', #3189, 1000.000000000000114 ) ;
#7395 = CARTESIAN_POINT ( 'NONE',  ( -24.15110854952566299, -134.0910177696405299, 49.99999999999997868 ) ) ;
#7396 = EDGE_CURVE ( 'NONE', #9491, #3983, #720, .T. ) ;
#7397 = ORIENTED_EDGE ( 'NONE', *, *, #817, .T. ) ;
#7398 =( LENGTH_UNIT ( ) NAMED_UNIT ( * ) SI_UNIT ( .MILLI., .METRE. ) );
#7399 = VECTOR ( 'NONE', #7539, 1000.000000000000000 ) ;
#7400 = DIRECTION ( 'NONE',  ( 0.000000000000000000, 0.000000000000000000, 1.000000000000000000 ) ) ;
#7401 = LINE ( 'NONE', #6550, #9904 ) ;
#7402 = DIRECTION ( 'NONE',  ( 0.000000000000000000, -0.000000000000000000, -1.000000000000000000 ) ) ;
#7403 = SURFACE_STYLE_USAGE ( .BOTH. , #4225 ) ;
#7404 = AXIS2_PLACEMENT_3D ( 'NONE', #1513, #851, #2884 ) ;
#7405 = CYLINDRICAL_SURFACE ( 'NONE', #9356, 3.999999999999993339 ) ;
#7406 = VERTEX_POINT ( 'NONE', #3624 ) ;
#7407 = AXIS2_PLACEMENT_3D ( 'NONE', #5203, #3727, #444 ) ;
#7408 = CARTESIAN_POINT ( 'NONE',  ( -18.34874108452141783, -140.1746510883711778, -97.78965767959371647 ) ) ;
#7409 = ADVANCED_FACE ( 'NONE', ( #9296 ), #2982, .F. ) ;
#7410 = ADVANCED_FACE ( 'NONE', ( #2767 ), #3257, .F. ) ;
#7411 = EDGE_CURVE ( 'NONE', #2989, #7514, #2190, .T. ) ;
#7412 = EDGE_LOOP ( 'NONE', ( #9174, #8854 ) ) ;
#7413 = DIRECTION ( 'NONE',  ( -1.000000000000000000, 0.000000000000000000, 0.000000000000000000 ) ) ;
#7414 = CARTESIAN_POINT ( 'NONE',  ( -2.293506896408097795, 126.8146633489777599, -25.00000000000000000 ) ) ;
#7415 = DIRECTION ( 'NONE',  ( 1.000000000000000000, -0.000000000000000000, -0.000000000000000000 ) ) ;
#7416 = DIRECTION ( 'NONE',  ( -0.000000000000000000, -0.000000000000000000, -1.000000000000000000 ) ) ;
#7417 = DIRECTION ( 'NONE',  ( -1.000000000000000000, 0.000000000000000000, -8.379529552680124346E-16 ) ) ;
#7418 = AXIS2_PLACEMENT_3D ( 'NONE', #3121, #3820, #9656 ) ;
#7419 =( REPRESENTATION_RELATIONSHIP ('NONE','NONE', #9007, #6561 ) REPRESENTATION_RELATIONSHIP_WITH_TRANSFORMATION ( #8026 )SHAPE_REPRESENTATION_RELATIONSHIP( ) );
#7420 = DIRECTION ( 'NONE',  ( 0.000000000000000000, 0.000000000000000000, 1.000000000000000000 ) ) ;
#7421 = VERTEX_POINT ( 'NONE', #6854 ) ;
#7422 = VERTEX_POINT ( 'NONE', #9399 ) ;
#7423 = EDGE_CURVE ( 'NONE', #6261, #6849, #7997, .T. ) ;
#7424 = AXIS2_PLACEMENT_3D ( 'NONE', #3384, #7413, #4071 ) ;
#7425 = ORIENTED_EDGE ( 'NONE', *, *, #4618, .T. ) ;
#7426 = EDGE_CURVE ( 'NONE', #7523, #4871, #1905, .T. ) ;
#7427 = DIRECTION ( 'NONE',  ( -0.000000000000000000, 1.000000000000000000, 0.000000000000000000 ) ) ;
#7428 = CARTESIAN_POINT ( 'NONE',  ( -47.94539818030328604, 155.5289575273811522, 0.000000000000000000 ) ) ;
#7429 = VECTOR ( 'NONE', #855, 1000.000000000000114 ) ;
#7430 = DIRECTION ( 'NONE',  ( 0.000000000000000000, -1.000000000000000000, 0.000000000000000000 ) ) ;
#7431 = ORIENTED_EDGE ( 'NONE', *, *, #6125, .F. ) ;
#7432 = DIRECTION ( 'NONE',  ( -0.6691306063588560171, -0.7431448254773961315, 0.000000000000000000 ) ) ;
#7433 = ORIENTED_EDGE ( 'NONE', *, *, #7301, .T. ) ;
#7434 = LINE ( 'NONE', #9021, #7429 ) ;
#7435 = CIRCLE ( 'NONE', #6074, 6.382478589986778417 ) ;
#7436 = ORIENTED_EDGE ( 'NONE', *, *, #6506, .F. ) ;
#7437 = EDGE_CURVE ( 'NONE', #4078, #8969, #3730, .T. ) ;
#7438 = DIRECTION ( 'NONE',  ( -1.000000000000000000, -0.000000000000000000, -0.000000000000000000 ) ) ;
#7439 = FACE_BOUND ( 'NONE', #6620, .T. ) ;
#7440 = CARTESIAN_POINT ( 'NONE',  ( -30.29350689640809335, 72.56966535057935630, 20.00000000000001066 ) ) ;
#7441 = DIRECTION ( 'NONE',  ( -0.000000000000000000, -0.000000000000000000, -1.000000000000000000 ) ) ;
#7442 = VECTOR ( 'NONE', #5129, 1000.000000000000000 ) ;
#7443 = DIRECTION ( 'NONE',  ( -1.000000000000000000, -0.000000000000000000, -8.379529552680125332E-16 ) ) ;
#7444 = ADVANCED_FACE ( 'NONE', ( #5209 ), #4111, .T. ) ;
#7445 = DIRECTION ( 'NONE',  ( 0.000000000000000000, 0.000000000000000000, 1.000000000000000000 ) ) ;
#7446 = EDGE_LOOP ( 'NONE', ( #4786, #7127, #3726, #3421 ) ) ;
#7447 = CARTESIAN_POINT ( 'NONE',  ( -7.293506896408097795, 80.56966535057935630, -28.00000000000001066 ) ) ;
#7448 = CONTEXT_DEPENDENT_SHAPE_REPRESENTATION ( #6733, #6446 ) ;
#7449 = ORIENTED_EDGE ( 'NONE', *, *, #3109, .T. ) ;
#7450 = CARTESIAN_POINT ( 'NONE',  ( -48.00000000000002132, -117.1457019118819005, 25.15769640663938134 ) ) ;
#7451 = EDGE_LOOP ( 'NONE', ( #9560, #4630, #9227, #10180 ) ) ;
#7452 =( NAMED_UNIT ( * ) PLANE_ANGLE_UNIT ( ) SI_UNIT ( $, .RADIAN. ) );
#7453 = ORIENTED_EDGE ( 'NONE', *, *, #4048, .F. ) ;
#7454 = DIRECTION ( 'NONE',  ( 0.000000000000000000, 0.000000000000000000, -1.000000000000000000 ) ) ;
#7455 = CARTESIAN_POINT ( 'NONE',  ( 0.3000000000000016542, 0.000000000000000000, 0.000000000000000000 ) ) ;
#7456 = DIRECTION ( 'NONE',  ( -1.000000000000000000, -0.000000000000000000, -0.000000000000000000 ) ) ;
#7457 = CARTESIAN_POINT ( 'NONE',  ( -40.00000000000002842, -135.1457019118818721, 39.99999999999997868 ) ) ;
#7458 = DIRECTION ( 'NONE',  ( -0.000000000000000000, -1.000000000000000000, -0.000000000000000000 ) ) ;
#7459 = ORIENTED_EDGE ( 'NONE', *, *, #1275, .T. ) ;
#7460 = LINE ( 'NONE', #3484, #5360 ) ;
#7461 = ORIENTED_EDGE ( 'NONE', *, *, #10385, .F. ) ;
#7462 = CARTESIAN_POINT ( 'NONE',  ( 25.15769640663940265, -117.1457019118819005, -48.00000000000002132 ) ) ;
#7463 = LINE ( 'NONE', #999, #9821 ) ;
#7464 = DIRECTION ( 'NONE',  ( 1.000000000000000000, 0.000000000000000000, 0.000000000000000000 ) ) ;
#7465 = CARTESIAN_POINT ( 'NONE',  ( -18.34874108452141783, -140.1746510883711778, 49.99999999999997868 ) ) ;
#7466 = DIRECTION ( 'NONE',  ( 0.000000000000000000, 1.000000000000000000, 0.000000000000000000 ) ) ;
#7467 = EDGE_CURVE ( 'NONE', #172, #1886, #2132, .T. ) ;
#7468 = ORIENTED_EDGE ( 'NONE', *, *, #9578, .F. ) ;
#7469 = AXIS2_PLACEMENT_3D ( 'NONE', #4327, #6068, #1937 ) ;
#7470 = EDGE_LOOP ( 'NONE', ( #10111, #9232 ) ) ;
#7471 = ORIENTED_EDGE ( 'NONE', *, *, #10283, .F. ) ;
#7472 = ORIENTED_EDGE ( 'NONE', *, *, #3313, .F. ) ;
#7473 = DIRECTION ( 'NONE',  ( 0.000000000000000000, 0.000000000000000000, 1.000000000000000000 ) ) ;
#7474 = DIRECTION ( 'NONE',  ( 6.106226635438360972E-16, -1.000000000000000000, 0.000000000000000000 ) ) ;
#7475 =( REPRESENTATION_RELATIONSHIP ('NONE','NONE', #9007, #1081 ) REPRESENTATION_RELATIONSHIP_WITH_TRANSFORMATION ( #5638 )SHAPE_REPRESENTATION_RELATIONSHIP( ) );
#7476 = CIRCLE ( 'NONE', #6296, 3.999999999999998668 ) ;
#7477 = DIRECTION ( 'NONE',  ( 1.000000000000000000, 0.000000000000000000, 0.000000000000000000 ) ) ;
#7478 = CARTESIAN_POINT ( 'NONE',  ( -31.74999999999995737, 6.123233995736766282E-16, -5.000000000000000000 ) ) ;
#7479 = ORIENTED_EDGE ( 'NONE', *, *, #6775, .F. ) ;
#7480 = EDGE_CURVE ( 'NONE', #4076, #4567, #557, .T. ) ;
#7481 = CARTESIAN_POINT ( 'NONE',  ( -1.071796769724492338, 0.000000000000000000, 0.000000000000000000 ) ) ;
#7482 = ADVANCED_FACE ( 'NONE', ( #4572 ), #7803, .F. ) ;
#7483 = EDGE_CURVE ( 'NONE', #1439, #8633, #8651, .T. ) ;
#7484 = VERTEX_POINT ( 'NONE', #1394 ) ;
#7485 = CARTESIAN_POINT ( 'NONE',  ( -2.293506896408101348, 150.5696653505793563, -10.98204862120179826 ) ) ;
#7486 = CIRCLE ( 'NONE', #2914, 7.000000000000016875 ) ;
#7487 = CIRCLE ( 'NONE', #7657, 0.2999999999999999334 ) ;
#7488 = ORIENTED_EDGE ( 'NONE', *, *, #4444, .F. ) ;
#7489 = PRODUCT_DEFINITION_CONTEXT ( 'detailed design', #770, 'design' ) ;
#7490 = CARTESIAN_POINT ( 'NONE',  ( 23.15769640663936713, -133.1457019118818721, 47.99999999999997868 ) ) ;
#7491 = CARTESIAN_POINT ( 'NONE',  ( 0.000000000000000000, -115.1457019118818863, 0.000000000000000000 ) ) ;
#7492 = CARTESIAN_POINT ( 'NONE',  ( -40.00000000000002842, -135.1457019118818721, 39.99999999999997868 ) ) ;
#7493 = DIRECTION ( 'NONE',  ( 1.000000000000000000, -0.000000000000000000, -0.000000000000000000 ) ) ;
#7494 = VECTOR ( 'NONE', #8220, 1000.000000000000000 ) ;
#7495 = DIRECTION ( 'NONE',  ( -0.7431448254773957984, 0.6691306063588565722, -0.000000000000000000 ) ) ;
#7496 = CARTESIAN_POINT ( 'NONE',  ( -21.44003972449640116, -143.0117419471019673, 6.332076144530967454 ) ) ;
#7497 = EDGE_CURVE ( 'NONE', #4536, #249, #5799, .T. ) ;
#7498 = ORIENTED_EDGE ( 'NONE', *, *, #9553, .F. ) ;
#7499 = LINE ( 'NONE', #4893, #1406 ) ;
#7500 = ORIENTED_EDGE ( 'NONE', *, *, #7765, .F. ) ;
#7501 = VECTOR ( 'NONE', #7743, 1000.000000000000000 ) ;
#7502 = DIRECTION ( 'NONE',  ( 1.000000000000000000, 0.000000000000000000, 0.000000000000000000 ) ) ;
#7503 = EDGE_LOOP ( 'NONE', ( #5614, #2058, #10115, #2127 ) ) ;
#7504 = CARTESIAN_POINT ( 'NONE',  ( -30.29350689640809335, 80.56966535057935630, 24.00000000000000711 ) ) ;
#7505 = CARTESIAN_POINT ( 'NONE',  ( -30.29350689640809335, 120.5696653505793705, 20.00000000000000711 ) ) ;
#7506 = DIRECTION ( 'NONE',  ( -1.000000000000000000, -0.000000000000000000, -0.000000000000000000 ) ) ;
#7507 = AXIS2_PLACEMENT_3D ( 'NONE', #472, #1317, #5233 ) ;
#7508 = CARTESIAN_POINT ( 'NONE',  ( 27.15769640663938489, -117.1457019118819005, -27.15769640663940976 ) ) ;
#7509 = DIRECTION ( 'NONE',  ( -1.000000000000000000, -0.000000000000000000, -0.000000000000000000 ) ) ;
#7510 = DIRECTION ( 'NONE',  ( 1.000000000000000000, 0.000000000000000000, 0.000000000000000000 ) ) ;
#7511 = ORIENTED_EDGE ( 'NONE', *, *, #1915, .T. ) ;
#7512 = DIRECTION ( 'NONE',  ( 0.000000000000000000, 0.000000000000000000, 1.000000000000000000 ) ) ;
#7513 = EDGE_CURVE ( 'NONE', #13, #2019, #4453, .T. ) ;
#7514 = VERTEX_POINT ( 'NONE', #1236 ) ;
#7515 = CARTESIAN_POINT ( 'NONE',  ( -16.29350689640809691, -140.1746510883711778, 7.500000000000000000 ) ) ;
#7516 = FACE_OUTER_BOUND ( 'NONE', #7446, .T. ) ;
#7517 = FACE_OUTER_BOUND ( 'NONE', #10400, .T. ) ;
#7518 = LINE ( 'NONE', #5868, #8011 ) ;
#7519 = DIRECTION ( 'NONE',  ( 0.000000000000000000, 0.000000000000000000, 1.000000000000000000 ) ) ;
#7520 = DIRECTION ( 'NONE',  ( -0.000000000000000000, 0.000000000000000000, 1.000000000000000000 ) ) ;
#7521 =( BOUNDED_CURVE ( )  B_SPLINE_CURVE ( 3, ( #9996, #3683, #8442, #8340 ),
 .UNSPECIFIED., .F., .F. ) 
 B_SPLINE_CURVE_WITH_KNOTS ( ( 4, 4 ),
 ( 4.712388980384689674, 7.853981633974482790 ),
 .UNSPECIFIED. ) 
 CURVE ( )  GEOMETRIC_REPRESENTATION_ITEM ( )  RATIONAL_B_SPLINE_CURVE ( ( 1.000000000000000000, 0.3333333333333333703, 0.3333333333333333703, 1.000000000000000000 ) ) 
 REPRESENTATION_ITEM ( '' )  );
#7522 = VECTOR ( 'NONE', #1923, 1000.000000000000000 ) ;
#7523 = VERTEX_POINT ( 'NONE', #7701 ) ;
#7524 = EDGE_LOOP ( 'NONE', ( #671, #1086, #1486, #7823, #4714, #7292, #6545, #6787 ) ) ;
#7525 = ORIENTED_EDGE ( 'NONE', *, *, #5544, .T. ) ;
#7526 = ADVANCED_FACE ( 'NONE', ( #447 ), #10144, .T. ) ;
#7527 = CARTESIAN_POINT ( 'NONE',  ( -30.29350689640809335, 120.5696653505793705, -27.99999999999999645 ) ) ;
#7528 = CIRCLE ( 'NONE', #2289, 4.024999999999997691 ) ;
#7529 = CARTESIAN_POINT ( 'NONE',  ( -16.26850689640809833, 140.5696653505793563, -10.90000000000000036 ) ) ;
#7530 = DIRECTION ( 'NONE',  ( -0.000000000000000000, 1.000000000000000000, -0.000000000000000000 ) ) ;
#7531 = CONICAL_SURFACE ( 'NONE', #9742, 6.499999999999964473, 0.7853981633974560506 ) ;
#7532 = ORIENTED_EDGE ( 'NONE', *, *, #9293, .F. ) ;
#7533 = DIRECTION ( 'NONE',  ( 0.000000000000000000, 0.000000000000000000, -1.000000000000000000 ) ) ;
#7534 = ORIENTED_EDGE ( 'NONE', *, *, #5008, .T. ) ;
#7535 = DIRECTION ( 'NONE',  ( 0.000000000000000000, 0.000000000000000000, 1.000000000000000000 ) ) ;
#7536 = CIRCLE ( 'NONE', #7371, 3.999999999999996447 ) ;
#7537 = VERTEX_POINT ( 'NONE', #752 ) ;
#7538 = EDGE_CURVE ( 'NONE', #10447, #9655, #10207, .T. ) ;
#7539 = DIRECTION ( 'NONE',  ( -0.6585271261848804070, 0.7525569905852197428, 0.000000000000000000 ) ) ;
#7540 = EDGE_CURVE ( 'NONE', #1359, #8958, #1405, .T. ) ;
#7541 = DIRECTION ( 'NONE',  ( 0.000000000000000000, 0.000000000000000000, -1.000000000000000000 ) ) ;
#7542 = EDGE_CURVE ( 'NONE', #4047, #3180, #1651, .T. ) ;
#7543 = DIRECTION ( 'NONE',  ( 0.000000000000000000, 0.000000000000000000, -1.000000000000000000 ) ) ;
#7544 = DIRECTION ( 'NONE',  ( 0.000000000000000000, 0.000000000000000000, -1.000000000000000000 ) ) ;
#7545 = FACE_BOUND ( 'NONE', #10427, .T. ) ;
#7546 = DIRECTION ( 'NONE',  ( -0.000000000000000000, -1.000000000000000000, -0.000000000000000000 ) ) ;
#7547 = VECTOR ( 'NONE', #8982, 1000.000000000000000 ) ;
#7548 = ORIENTED_EDGE ( 'NONE', *, *, #5977, .F. ) ;
#7549 = DIRECTION ( 'NONE',  ( -1.000000000000000000, 0.000000000000000000, -0.000000000000000000 ) ) ;
#7550 = EDGE_LOOP ( 'NONE', ( #6016, #7338, #3210, #9417 ) ) ;
#7551 = CIRCLE ( 'NONE', #4833, 5.000000000000000888 ) ;
#7552 = LINE ( 'NONE', #304, #10072 ) ;
#7553 = ORIENTED_EDGE ( 'NONE', *, *, #5872, .T. ) ;
#7554 = AXIS2_PLACEMENT_3D ( 'NONE', #9191, #396, #3625 ) ;
#7555 = ADVANCED_FACE ( 'NONE', ( #3835 ), #4727, .F. ) ;
#7556 = ORIENTED_EDGE ( 'NONE', *, *, #9788, .T. ) ;
#7557 = FACE_OUTER_BOUND ( 'NONE', #1498, .T. ) ;
#7558 = DIRECTION ( 'NONE',  ( 0.000000000000000000, 0.000000000000000000, -1.000000000000000000 ) ) ;
#7559 = DIRECTION ( 'NONE',  ( 0.000000000000000000, 0.000000000000000000, 1.000000000000000000 ) ) ;
#7560 = AXIS2_PLACEMENT_3D ( 'NONE', #2820, #10309, #9510 ) ;
#7561 =( NAMED_UNIT ( * ) PLANE_ANGLE_UNIT ( ) SI_UNIT ( $, .RADIAN. ) );
#7562 = ORIENTED_EDGE ( 'NONE', *, *, #1902, .T. ) ;
#7563 = CARTESIAN_POINT ( 'NONE',  ( -23.15769640663940976, -117.1457019118819005, 47.99999999999997868 ) ) ;
#7564 = CIRCLE ( 'NONE', #8241, 47.56532671630425568 ) ;
#7565 = CARTESIAN_POINT ( 'NONE',  ( 0.000000000000000000, 0.000000000000000000, 0.000000000000000000 ) ) ;
#7566 = ORIENTED_EDGE ( 'NONE', *, *, #4605, .T. ) ;
#7567 = PLANE ( 'NONE',  #1981 ) ;
#7568 = AXIS2_PLACEMENT_3D ( 'NONE', #885, #6664, #3327 ) ;
#7569 = EDGE_LOOP ( 'NONE', ( #340, #5978, #9234, #9832 ) ) ;
#7570 = CARTESIAN_POINT ( 'NONE',  ( -30.29350689640809335, 2.445795361565304815E-15, -20.00000000000002132 ) ) ;
#7571 = DIRECTION ( 'NONE',  ( -1.000000000000000000, 0.000000000000000000, -0.000000000000000000 ) ) ;
#7572 = CARTESIAN_POINT ( 'NONE',  ( 99.80027788547049283, -145.1457019118819005, 30.00000000000000355 ) ) ;
#7573 = AXIS2_PLACEMENT_3D ( 'NONE', #1315, #8730, #3058 ) ;
#7574 = DIRECTION ( 'NONE',  ( 0.000000000000000000, 0.000000000000000000, 1.000000000000000000 ) ) ;
#7575 = PLANE ( 'NONE',  #8039 ) ;
#7576 = CARTESIAN_POINT ( 'NONE',  ( -2.293506896408097795, 126.8146633489777599, 25.00000000000000355 ) ) ;
#7577 = EDGE_CURVE ( 'NONE', #5461, #2007, #5622, .T. ) ;
#7578 = CIRCLE ( 'NONE', #5537, 6.382478589986750883 ) ;
#7579 = ORIENTED_EDGE ( 'NONE', *, *, #1711, .T. ) ;
#7580 = ORIENTED_EDGE ( 'NONE', *, *, #6644, .T. ) ;
#7581 = VECTOR ( 'NONE', #906, 1000.000000000000000 ) ;
#7582 = ORIENTED_EDGE ( 'NONE', *, *, #8703, .T. ) ;
#7583 = DIRECTION ( 'NONE',  ( -1.000000000000000000, -0.000000000000000000, -0.000000000000000000 ) ) ;
#7584 = CARTESIAN_POINT ( 'NONE',  ( 37.22511195853868315, -116.3672949040186779, -25.00000000000000355 ) ) ;
#7585 = AXIS2_PLACEMENT_3D ( 'NONE', #4918, #8161, #5879 ) ;
#7586 = CARTESIAN_POINT ( 'NONE',  ( -161.3589532509997468, 266.5515548974023545, 0.000000000000000000 ) ) ;
#7587 = SHAPE_REPRESENTATION ( 'Metal Rod', ( #4601 ), #2278 ) ;
#7588 = DIRECTION ( 'NONE',  ( -1.000000000000000000, 0.000000000000000000, 0.000000000000000000 ) ) ;
#7589 = ORIENTED_EDGE ( 'NONE', *, *, #2521, .F. ) ;
#7590 = CARTESIAN_POINT ( 'NONE',  ( -27.15769640663940976, -115.1457019118818863, 23.15769640663938134 ) ) ;
#7591 = EDGE_LOOP ( 'NONE', ( #9394, #7354, #4729, #2159 ) ) ;
#7592 = DIRECTION ( 'NONE',  ( -0.000000000000000000, 1.000000000000000000, 1.224646799147353207E-16 ) ) ;
#7593 = EDGE_CURVE ( 'NONE', #6151, #6524, #2752, .T. ) ;
#7594 = CIRCLE ( 'NONE', #983, 2.000000000000001776 ) ;
#7595 = ORIENTED_EDGE ( 'NONE', *, *, #5069, .T. ) ;
#7596 = CIRCLE ( 'NONE', #8946, 7.725331121244574994 ) ;
#7597 = EDGE_LOOP ( 'NONE', ( #2049, #4582, #9470, #951 ) ) ;
#7598 = DIRECTION ( 'NONE',  ( 0.000000000000000000, -1.000000000000000000, 1.222897680782651471E-16 ) ) ;
#7599 = CARTESIAN_POINT ( 'NONE',  ( 27.15769640663936713, -133.1457019118818721, 27.15769640663938489 ) ) ;
#7600 = DIRECTION ( 'NONE',  ( -0.000000000000000000, 1.000000000000000000, 0.000000000000000000 ) ) ;
#7601 = CARTESIAN_POINT ( 'NONE',  ( -48.00000000000002842, -115.1457019118818863, 23.15769640663938134 ) ) ;
#7602 = DIRECTION ( 'NONE',  ( 0.000000000000000000, -1.000000000000000000, 0.000000000000000000 ) ) ;
#7603 = ORIENTED_EDGE ( 'NONE', *, *, #6447, .T. ) ;
#7604 = TOROIDAL_SURFACE ( 'NONE', #3032, 11.15107097094592881, 2.515249034521771510 ) ;
#7605 = CARTESIAN_POINT ( 'NONE',  ( -43.93820948810023452, -4.000000000000000888, -4.898587196589413815E-16 ) ) ;
#7606 = ADVANCED_FACE ( 'NONE', ( #4874, #1503 ), #7964, .T. ) ;
#7607 = ADVANCED_FACE ( 'NONE', ( #802 ), #6814, .T. ) ;
#7608 = EDGE_LOOP ( 'NONE', ( #4592, #6631, #4868, #7842 ) ) ;
#7609 = CARTESIAN_POINT ( 'NONE',  ( 2.108096605167896559E-14, -115.1457019118818863, -25.15769640663943107 ) ) ;
#7610 = ORIENTED_EDGE ( 'NONE', *, *, #6573, .F. ) ;
#7611 = CARTESIAN_POINT ( 'NONE',  ( 0.3000000000000016542, 0.000000000000000000, 0.000000000000000000 ) ) ;
#7612 = DIRECTION ( 'NONE',  ( 0.000000000000000000, 0.000000000000000000, 1.000000000000000000 ) ) ;
#7613 =( LENGTH_UNIT ( ) NAMED_UNIT ( * ) SI_UNIT ( .MILLI., .METRE. ) );
#7614 = ORIENTED_EDGE ( 'NONE', *, *, #6759, .F. ) ;
#7615 = CARTESIAN_POINT ( 'NONE',  ( -27.15769640663939555, -117.1457019118819005, -27.15769640663944173 ) ) ;
#7616 = ADVANCED_FACE ( 'NONE', ( #5519 ), #394, .F. ) ;
#7617 = EDGE_CURVE ( 'NONE', #9114, #1889, #3095, .T. ) ;
#7618 = EDGE_CURVE ( 'NONE', #382, #7686, #3591, .T. ) ;
#7619 = ORIENTED_EDGE ( 'NONE', *, *, #1772, .T. ) ;
#7620 = CARTESIAN_POINT ( 'NONE',  ( 0.000000000000000000, 0.000000000000000000, 0.000000000000000000 ) ) ;
#7621 = ORIENTED_EDGE ( 'NONE', *, *, #7098, .F. ) ;
#7622 = PLANE ( 'NONE',  #5016 ) ;
#7623 = ORIENTED_EDGE ( 'NONE', *, *, #9691, .T. ) ;
#7624 = DIRECTION ( 'NONE',  ( -8.379529552680124346E-16, 0.000000000000000000, 1.000000000000000000 ) ) ;
#7625 = DIRECTION ( 'NONE',  ( -1.000000000000000000, -0.000000000000000000, -0.000000000000000000 ) ) ;
#7626 = DIRECTION ( 'NONE',  ( 1.000000000000000000, 0.000000000000000000, 0.000000000000000000 ) ) ;
#7627 = LINE ( 'NONE', #1210, #3982 ) ;
#7628 = DIRECTION ( 'NONE',  ( 9.101836848464095537E-17, 0.000000000000000000, 1.000000000000000000 ) ) ;
#7629 = ADVANCED_FACE ( 'NONE', ( #3137 ), #2390, .T. ) ;
#7630 = ORIENTED_EDGE ( 'NONE', *, *, #9849, .F. ) ;
#7631 = ORIENTED_EDGE ( 'NONE', *, *, #7513, .F. ) ;
#7632 = DIRECTION ( 'NONE',  ( 1.000000000000000000, 0.000000000000000000, 0.000000000000000000 ) ) ;
#7633 = ADVANCED_FACE ( 'NONE', ( #5670 ), #3237, .F. ) ;
#7634 = CARTESIAN_POINT ( 'NONE',  ( -48.00000000000002132, -135.1457019118818721, -27.15769640663945950 ) ) ;
#7635 = DIRECTION ( 'NONE',  ( 0.000000000000000000, 1.000000000000000000, 0.000000000000000000 ) ) ;
#7636 = VECTOR ( 'NONE', #6190, 1000.000000000000000 ) ;
#7637 = ORIENTED_EDGE ( 'NONE', *, *, #6493, .F. ) ;
#7638 = CARTESIAN_POINT ( 'NONE',  ( -127.7900974404101930, 225.7464258663465557, 0.000000000000000000 ) ) ;
#7639 = VERTEX_POINT ( 'NONE', #6370 ) ;
#7640 = TOROIDAL_SURFACE ( 'NONE', #7649, 4.000000000000000000, 2.000000000000000000 ) ;
#7641 = ORIENTED_EDGE ( 'NONE', *, *, #2503, .F. ) ;
#7642 = AXIS2_PLACEMENT_3D ( 'NONE', #3728, #1126, #4519 ) ;
#7643 = CARTESIAN_POINT ( 'NONE',  ( -47.94539818030328604, 85.52895752738115220, 0.000000000000000000 ) ) ;
#7644 = EDGE_CURVE ( 'NONE', #3341, #3030, #5791, .T. ) ;
#7645 = CARTESIAN_POINT ( 'NONE',  ( -30.29350689640809335, 120.5696653505793705, -24.00000000000000711 ) ) ;
#7646 = DIRECTION ( 'NONE',  ( -0.6691306063588565722, -0.7431448254773956874, 0.000000000000000000 ) ) ;
#7647 = DIRECTION ( 'NONE',  ( -1.000000000000000000, 0.000000000000000000, -8.379529552680125332E-16 ) ) ;
#7648 = PLANE ( 'NONE',  #449 ) ;
#7649 = AXIS2_PLACEMENT_3D ( 'NONE', #2175, #7056, #10292 ) ;
#7650 = ORIENTED_EDGE ( 'NONE', *, *, #118, .F. ) ;
#7651 = CIRCLE ( 'NONE', #6115, 4.000000000000000000 ) ;
#7652 = LINE ( 'NONE', #2771, #10021 ) ;
#7653 = ORIENTED_EDGE ( 'NONE', *, *, #7749, .F. ) ;
#7654 = LINE ( 'NONE', #6061, #6409 ) ;
#7655 = ORIENTED_EDGE ( 'NONE', *, *, #7706, .F. ) ;
#7656 = AXIS2_PLACEMENT_3D ( 'NONE', #3364, #2510, #972 ) ;
#7657 = AXIS2_PLACEMENT_3D ( 'NONE', #9747, #8299, #6499 ) ;
#7658 = EDGE_CURVE ( 'NONE', #1931, #941, #6469, .T. ) ;
#7659 = CARTESIAN_POINT ( 'NONE',  ( 39.99999999999998579, -135.1707019118818778, -44.00000000000002132 ) ) ;
#7660 = DIRECTION ( 'NONE',  ( -1.000000000000000000, 0.000000000000000000, 0.000000000000000000 ) ) ;
#7661 = FACE_OUTER_BOUND ( 'NONE', #10437, .T. ) ;
#7662 = DIRECTION ( 'NONE',  ( 0.000000000000000000, -0.9961946980917458783, 0.08715574274765483520 ) ) ;
#7663 = ORIENTED_EDGE ( 'NONE', *, *, #3225, .F. ) ;
#7664 = CARTESIAN_POINT ( 'NONE',  ( -47.94539818030330025, 150.5696653505793563, 0.000000000000000000 ) ) ;
#7665 = VECTOR ( 'NONE', #8912, 1000.000000000000000 ) ;
#7666 = VERTEX_POINT ( 'NONE', #7916 ) ;
#7667 =( NAMED_UNIT ( * ) PLANE_ANGLE_UNIT ( ) SI_UNIT ( $, .RADIAN. ) );
#7668 = ORIENTED_EDGE ( 'NONE', *, *, #8865, .T. ) ;
#7669 = LINE ( 'NONE', #10058, #459 ) ;
#7670 = ORIENTED_EDGE ( 'NONE', *, *, #4816, .T. ) ;
#7671 = LINE ( 'NONE', #7570, #6701 ) ;
#7672 = EDGE_CURVE ( 'NONE', #6356, #3441, #9871, .T. ) ;
#7673 = CARTESIAN_POINT ( 'NONE',  ( 42.22511195853868315, -135.1457019118818721, 30.00000000000000355 ) ) ;
#7674 = EDGE_CURVE ( 'NONE', #8078, #2621, #3291, .T. ) ;
#7675 = EDGE_CURVE ( 'NONE', #1889, #5302, #956, .T. ) ;
#7676 = LINE ( 'NONE', #1046, #9134 ) ;
#7677 = LINE ( 'NONE', #2743, #1247 ) ;
#7678 = CARTESIAN_POINT ( 'NONE',  ( -47.94539818030330025, 150.5446653505793790, 0.000000000000000000 ) ) ;
#7679 = CARTESIAN_POINT ( 'NONE',  ( 39.99999999999998579, -135.1457019118818721, -40.00000000000002132 ) ) ;
#7680 = APPLICATION_CONTEXT ( 'automotive_design' ) ;
#7681 = EDGE_LOOP ( 'NONE', ( #3723, #5731, #2530, #2597 ) ) ;
#7682 = ORIENTED_EDGE ( 'NONE', *, *, #1026, .T. ) ;
#7683 = CIRCLE ( 'NONE', #8531, 47.56532671630425568 ) ;
#7684 = LINE ( 'NONE', #3817, #783 ) ;
#7685 = AXIS2_PLACEMENT_3D ( 'NONE', #3586, #8460, #8355 ) ;
#7686 = VERTEX_POINT ( 'NONE', #4243 ) ;
#7687 = CYLINDRICAL_SURFACE ( 'NONE', #3023, 4.000000000000000000 ) ;
#7688 = CARTESIAN_POINT ( 'NONE',  ( -47.94539818030328604, 70.52895752738115220, 4.000000000000000000 ) ) ;
#7689 = EDGE_CURVE ( 'NONE', #9794, #415, #6136, .T. ) ;
#7690 = PLANE ( 'NONE',  #9027 ) ;
#7691 = DIRECTION ( 'NONE',  ( -0.6585271261848804070, 0.7525569905852197428, 0.000000000000000000 ) ) ;
#7692 = CIRCLE ( 'NONE', #9564, 4.025000000000000355 ) ;
#7693 = ORIENTED_EDGE ( 'NONE', *, *, #2905, .F. ) ;
#7694 = EDGE_LOOP ( 'NONE', ( #3531, #7156 ) ) ;
#7695 = AXIS2_PLACEMENT_3D ( 'NONE', #9030, #9678, #973 ) ;
#7696 = ORIENTED_EDGE ( 'NONE', *, *, #8449, .T. ) ;
#7697 = ORIENTED_EDGE ( 'NONE', *, *, #8314, .T. ) ;
#7698 = LINE ( 'NONE', #6049, #9796 ) ;
#7699 = CARTESIAN_POINT ( 'NONE',  ( -23.15769640663940976, -115.1457019118818863, 49.99999999999997868 ) ) ;
#7700 = CARTESIAN_POINT ( 'NONE',  ( -40.99999999999999289, -5.556536133988210224E-16, 4.000000000000005329 ) ) ;
#7701 = CARTESIAN_POINT ( 'NONE',  ( 23.15769640663936357, -115.1457019118818863, 27.15769640663938489 ) ) ;
#7702 = CARTESIAN_POINT ( 'NONE',  ( 26.00000000000000355, 0.000000000000000000, 0.000000000000000000 ) ) ;
#7703 = AXIS2_PLACEMENT_3D ( 'NONE', #1383, #5103, #8339 ) ;
#7704 = ORIENTED_EDGE ( 'NONE', *, *, #615, .F. ) ;
#7705 = CARTESIAN_POINT ( 'NONE',  ( -7.293506896408097795, 72.08684478514408056, -28.00000000000001421 ) ) ;
#7706 = EDGE_CURVE ( 'NONE', #382, #8839, #5034, .T. ) ;
#7707 = PLANE ( 'NONE',  #5568 ) ;
#7708 = LINE ( 'NONE', #3632, #3512 ) ;
#7709 = VECTOR ( 'NONE', #309, 1000.000000000000000 ) ;
#7710 = DIRECTION ( 'NONE',  ( 0.000000000000000000, 1.000000000000000000, 0.000000000000000000 ) ) ;
#7711 = CARTESIAN_POINT ( 'NONE',  ( 37.46742560152671331, -135.0531259799080033, 26.54270448881459643 ) ) ;
#7712 = DIRECTION ( 'NONE',  ( -1.000000000000000000, -0.000000000000000000, -0.000000000000000000 ) ) ;
#7713 = FACE_OUTER_BOUND ( 'NONE', #7819, .T. ) ;
#7714 = EDGE_LOOP ( 'NONE', ( #2060, #4813, #9775, #2263 ) ) ;
#7715 = CARTESIAN_POINT ( 'NONE',  ( -2.293506896408097795, 120.5696653505793705, -28.00000000000000355 ) ) ;
#7716 = CIRCLE ( 'NONE', #6015, 4.000000000000003553 ) ;
#7717 = ORIENTED_EDGE ( 'NONE', *, *, #757, .T. ) ;
#7718 =( NAMED_UNIT ( * ) PLANE_ANGLE_UNIT ( ) SI_UNIT ( $, .RADIAN. ) );
#7719 = EDGE_CURVE ( 'NONE', #1403, #7054, #5772, .T. ) ;
#7720 = ORIENTED_EDGE ( 'NONE', *, *, #9362, .F. ) ;
#7721 = VECTOR ( 'NONE', #6323, 1000.000000000000000 ) ;
#7722 = CARTESIAN_POINT ( 'NONE',  ( -2.293506896408097795, 37.08684478514406635, 30.00000000000000355 ) ) ;
#7723 = ORIENTED_EDGE ( 'NONE', *, *, #8806, .T. ) ;
#7724 = ORIENTED_EDGE ( 'NONE', *, *, #4294, .F. ) ;
#7725 = DIRECTION ( 'NONE',  ( 0.000000000000000000, 1.000000000000000000, 0.000000000000000000 ) ) ;
#7726 = LINE ( 'NONE', #4394, #7824 ) ;
#7727 = VECTOR ( 'NONE', #8684, 1000.000000000000000 ) ;
#7728 = SURFACE_STYLE_FILL_AREA ( #1103 ) ;
#7729 = LINE ( 'NONE', #323, #2424 ) ;
#7730 = CARTESIAN_POINT ( 'NONE',  ( -27.15769640663940976, -133.1457019118818721, 27.15769640663938489 ) ) ;
#7731 = VECTOR ( 'NONE', #2166, 1000.000000000000000 ) ;
#7732 = FACE_BOUND ( 'NONE', #2407, .T. ) ;
#7733 = ORIENTED_EDGE ( 'NONE', *, *, #1324, .T. ) ;
#7734 = EDGE_CURVE ( 'NONE', #4613, #7406, #900, .T. ) ;
#7735 = EDGE_LOOP ( 'NONE', ( #7772, #7154 ) ) ;
#7736 = VECTOR ( 'NONE', #2529, 1000.000000000000000 ) ;
#7737 = EDGE_CURVE ( 'NONE', #6362, #2500, #66, .T. ) ;
#7738 = DIRECTION ( 'NONE',  ( -0.7431448254773957984, 0.6691306063588565722, -0.000000000000000000 ) ) ;
#7739 = MECHANICAL_DESIGN_GEOMETRIC_PRESENTATION_REPRESENTATION (  '', ( #3509 ), #7909 ) ;
#7740 = EDGE_LOOP ( 'NONE', ( #3344, #5419 ) ) ;
#7741 = CARTESIAN_POINT ( 'NONE',  ( -39.00428932080996702, -3.095342794014893428, -1.752073144804227933 ) ) ;
#7742 = CARTESIAN_POINT ( 'NONE',  ( -47.94539818030330025, 90.52895752738122326, 0.000000000000000000 ) ) ;
#7743 = DIRECTION ( 'NONE',  ( -1.000000000000000000, 0.000000000000000000, 1.137729606058012035E-16 ) ) ;
#7744 = LINE ( 'NONE', #3720, #8250 ) ;
#7745 = CARTESIAN_POINT ( 'NONE',  ( -43.94539818030328604, 155.5289575273811522, 0.000000000000000000 ) ) ;
#7746 = ORIENTED_EDGE ( 'NONE', *, *, #4655, .T. ) ;
#7747 = ORIENTED_EDGE ( 'NONE', *, *, #9228, .T. ) ;
#7748 = EDGE_CURVE ( 'NONE', #7894, #3749, #1012, .T. ) ;
#7749 = EDGE_CURVE ( 'NONE', #2514, #5655, #7166, .T. ) ;
#7750 = EDGE_CURVE ( 'NONE', #1613, #3068, #4087, .T. ) ;
#7751 = AXIS2_PLACEMENT_3D ( 'NONE', #6579, #7473, #848 ) ;
#7752 = ORIENTED_EDGE ( 'NONE', *, *, #5916, .F. ) ;
#7753 = ORIENTED_EDGE ( 'NONE', *, *, #2429, .F. ) ;
#7754 = CARTESIAN_POINT ( 'NONE',  ( -21.29350689640810401, 105.5289575273812233, 54.43095569077609497 ) ) ;
#7755 = CARTESIAN_POINT ( 'NONE',  ( -16.29350689640809691, -115.1457019118818863, 23.72119897386845722 ) ) ;
#7756 = CARTESIAN_POINT ( 'NONE',  ( -30.29350689640809335, 80.56966535057935630, -28.00000000000000355 ) ) ;
#7757 = DIRECTION ( 'NONE',  ( 1.049727191138617710E-16, -0.5150380749100554878, 0.8571673007021115565 ) ) ;
#7758 = CARTESIAN_POINT ( 'NONE',  ( -30.29350689640809335, 120.5696653505793705, -20.00000000000000711 ) ) ;
#7759 = VECTOR ( 'NONE', #5401, 1000.000000000000000 ) ;
#7760 = ORIENTED_EDGE ( 'NONE', *, *, #8952, .T. ) ;
#7761 = CARTESIAN_POINT ( 'NONE',  ( -2.293506896408097795, 80.56966535057935630, 20.00000000000000711 ) ) ;
#7762 = ADVANCED_FACE ( 'NONE', ( #2601 ), #228, .T. ) ;
#7763 = DIRECTION ( 'NONE',  ( -9.776117811460147207E-16, 0.000000000000000000, 1.000000000000000000 ) ) ;
#7764 = AXIS2_PLACEMENT_3D ( 'NONE', #6934, #1156, #6021 ) ;
#7765 = EDGE_CURVE ( 'NONE', #1117, #716, #8853, .T. ) ;
#7766 = CARTESIAN_POINT ( 'NONE',  ( -30.29350689640809335, 140.5696653505793563, -20.00000000000000355 ) ) ;
#7767 = CIRCLE ( 'NONE', #9815, 3.999999999999993339 ) ;
#7768 = DIRECTION ( 'NONE',  ( -0.000000000000000000, 1.000000000000000000, -0.000000000000000000 ) ) ;
#7769 = CARTESIAN_POINT ( 'NONE',  ( -30.29350689640809335, 112.5696653505793705, 20.00000000000000711 ) ) ;
#7770 = ORIENTED_EDGE ( 'NONE', *, *, #9304, .T. ) ;
#7771 = DIRECTION ( 'NONE',  ( 0.000000000000000000, 0.000000000000000000, 1.000000000000000000 ) ) ;
#7772 = ORIENTED_EDGE ( 'NONE', *, *, #3980, .T. ) ;
#7773 = CARTESIAN_POINT ( 'NONE',  ( -36.29350689640811822, 120.5696653505793279, -20.00000000000001066 ) ) ;
#7774 = VERTEX_POINT ( 'NONE', #8323 ) ;
#7775 = DIRECTION ( 'NONE',  ( -0.000000000000000000, -1.000000000000000000, -0.000000000000000000 ) ) ;
#7776 = ORIENTED_EDGE ( 'NONE', *, *, #3611, .T. ) ;
#7777 = ORIENTED_EDGE ( 'NONE', *, *, #8597, .T. ) ;
#7778 = CARTESIAN_POINT ( 'NONE',  ( -2.293506896408097795, 147.5696653505793279, -25.00000000000000355 ) ) ;
#7779 = DIRECTION ( 'NONE',  ( 0.6691306063588561281, 0.7431448254773961315, 0.000000000000000000 ) ) ;
#7780 = ORIENTED_EDGE ( 'NONE', *, *, #31, .T. ) ;
#7781 = DIRECTION ( 'NONE',  ( 1.000000000000000000, 0.000000000000000000, 0.000000000000000000 ) ) ;
#7782 = DIRECTION ( 'NONE',  ( 1.000000000000000000, 0.000000000000000000, 0.000000000000000000 ) ) ;
#7783 = LINE ( 'NONE', #10229, #7636 ) ;
#7784 = COLOUR_RGB ( '',0.7921568627450980005, 0.8196078431372548767, 0.9333333333333333481 ) ;
#7785 = VERTEX_POINT ( 'NONE', #7529 ) ;
#7786 = DIRECTION ( 'NONE',  ( 0.000000000000000000, 0.000000000000000000, 1.000000000000000000 ) ) ;
#7787 = ORIENTED_EDGE ( 'NONE', *, *, #8696, .F. ) ;
#7788 = DIRECTION ( 'NONE',  ( 0.000000000000000000, -1.000000000000000000, -1.431206729101514631E-16 ) ) ;
#7789 = ORIENTED_EDGE ( 'NONE', *, *, #3594, .T. ) ;
#7790 = CARTESIAN_POINT ( 'NONE',  ( 10.26554134690924691, 90.52895752738122326, 7.749999999999998224 ) ) ;
#7791 = ADVANCED_FACE ( 'NONE', ( #1061 ), #2589, .F. ) ;
#7792 = CARTESIAN_POINT ( 'NONE',  ( -3.173844575093148990, 105.5289575273812233, 10.90000000000000036 ) ) ;
#7793 = CARTESIAN_POINT ( 'NONE',  ( -3.173844575093148990, 150.5696653505793563, 10.90000000000000036 ) ) ;
#7794 = ORIENTED_EDGE ( 'NONE', *, *, #7806, .T. ) ;
#7795 = ORIENTED_EDGE ( 'NONE', *, *, #7981, .T. ) ;
#7796 = PRODUCT_DEFINITION_SHAPE ( 'NONE', 'NONE',  #8329 ) ;
#7797 = ORIENTED_EDGE ( 'NONE', *, *, #9887, .T. ) ;
#7798 = ORIENTED_EDGE ( 'NONE', *, *, #1009, .T. ) ;
#7799 = CARTESIAN_POINT ( 'NONE',  ( -23.15769640663940976, -117.1457019118819005, 49.99999999999997868 ) ) ;
#7800 = CARTESIAN_POINT ( 'NONE',  ( 80.08610854271792334, 54.73418909528891874, 30.00000000000000355 ) ) ;
#7801 = AXIS2_PLACEMENT_3D ( 'NONE', #4901, #43, #9960 ) ;
#7802 = DIRECTION ( 'NONE',  ( -1.000000000000000000, 0.000000000000000000, -8.379529552680125332E-16 ) ) ;
#7803 = CYLINDRICAL_SURFACE ( 'NONE', #4275, 7.500000000000000000 ) ;
#7804 = EDGE_CURVE ( 'NONE', #8577, #8659, #3503, .T. ) ;
#7805 = ADVANCED_FACE ( 'NONE', ( #9772 ), #8512, .F. ) ;
#7806 = EDGE_CURVE ( 'NONE', #1913, #1439, #7174, .T. ) ;
#7807 = DIRECTION ( 'NONE',  ( 0.000000000000000000, -1.000000000000000000, 0.000000000000000000 ) ) ;
#7808 = ORIENTED_EDGE ( 'NONE', *, *, #1687, .T. ) ;
#7809 = CARTESIAN_POINT ( 'NONE',  ( -27.15769640663939555, -133.1457019118818721, -27.15769640663944173 ) ) ;
#7810 = VECTOR ( 'NONE', #9514, 1000.000000000000000 ) ;
#7811 = CIRCLE ( 'NONE', #9859, 7.728925574020643730 ) ;
#7812 = LINE ( 'NONE', #10152, #1340 ) ;
#7813 = ORIENTED_EDGE ( 'NONE', *, *, #4310, .T. ) ;
#7814 = TOROIDAL_SURFACE ( 'NONE', #3242, -39.11828581851394659, 47.56532671630426989 ) ;
#7815 = EDGE_CURVE ( 'NONE', #7120, #8465, #7321, .T. ) ;
#7816 = DIRECTION ( 'NONE',  ( -0.000000000000000000, -0.000000000000000000, 1.000000000000000000 ) ) ;
#7817 = DIRECTION ( 'NONE',  ( 1.000000000000000000, 0.000000000000000000, 0.000000000000000000 ) ) ;
#7818 = DIRECTION ( 'NONE',  ( -0.000000000000000000, -1.000000000000000000, -0.000000000000000000 ) ) ;
#7819 = EDGE_LOOP ( 'NONE', ( #2181, #1996, #6666, #7039 ) ) ;
#7820 = DIRECTION ( 'NONE',  ( -0.000000000000000000, 1.000000000000000000, -0.000000000000000000 ) ) ;
#7821 = ORIENTED_EDGE ( 'NONE', *, *, #10425, .T. ) ;
#7822 = APPLICATION_PROTOCOL_DEFINITION ( 'draft international standard', 'automotive_design', 1998, #7882 ) ;
#7823 = ORIENTED_EDGE ( 'NONE', *, *, #4238, .F. ) ;
#7824 = VECTOR ( 'NONE', #2791, 1000.000000000000114 ) ;
#7825 = DIRECTION ( 'NONE',  ( -1.277197683604454965E-16, 1.000000000000000000, -0.000000000000000000 ) ) ;
#7826 = ORIENTED_EDGE ( 'NONE', *, *, #401, .T. ) ;
#7827 = ORIENTED_EDGE ( 'NONE', *, *, #8411, .T. ) ;
#7828 = CARTESIAN_POINT ( 'NONE',  ( -20.14472382240650816, -141.8229441850657508, 25.87097612368018673 ) ) ;
#7829 = CARTESIAN_POINT ( 'NONE',  ( -23.15769640663937423, -117.1457019118819005, -48.00000000000002132 ) ) ;
#7830 = ORIENTED_EDGE ( 'NONE', *, *, #6913, .T. ) ;
#7831 = CARTESIAN_POINT ( 'NONE',  ( -31.74999999999995737, 0.000000000000000000, 0.000000000000000000 ) ) ;
#7832 = LINE ( 'NONE', #7148, #907 ) ;
#7833 = DIRECTION ( 'NONE',  ( 0.000000000000000000, 0.000000000000000000, -1.000000000000000000 ) ) ;
#7834 = AXIS2_PLACEMENT_3D ( 'NONE', #8285, #6692, #9133 ) ;
#7835 = FACE_BOUND ( 'NONE', #4917, .T. ) ;
#7836 = CIRCLE ( 'NONE', #5937, 2.999999999999999556 ) ;
#7837 = DIRECTION ( 'NONE',  ( 0.000000000000000000, -1.000000000000000000, -9.100899318238123202E-17 ) ) ;
#7838 = EDGE_CURVE ( 'NONE', #5742, #7514, #3268, .T. ) ;
#7839 = ORIENTED_EDGE ( 'NONE', *, *, #4462, .F. ) ;
#7840 = CARTESIAN_POINT ( 'NONE',  ( 27.15769640663938489, -117.1457019118819005, -23.15769640663940976 ) ) ;
#7841 = VECTOR ( 'NONE', #10345, 1000.000000000000000 ) ;
#7842 = ORIENTED_EDGE ( 'NONE', *, *, #6377, .F. ) ;
#7843 = CARTESIAN_POINT ( 'NONE',  ( 3.000000000000000000, 1.467624384280025174, -2.542000000000001592 ) ) ;
#7844 = DIRECTION ( 'NONE',  ( 0.000000000000000000, 0.000000000000000000, -1.000000000000000000 ) ) ;
#7845 = CARTESIAN_POINT ( 'NONE',  ( 37.22511195853868315, -116.3672949040187063, 25.00000000000000000 ) ) ;
#7846 = CARTESIAN_POINT ( 'NONE',  ( -23.15769640663937423, -135.1457019118818721, -48.00000000000002132 ) ) ;
#7847 = CYLINDRICAL_SURFACE ( 'NONE', #8368, 4.999999999999995559 ) ;
#7848 = VERTEX_POINT ( 'NONE', #4976 ) ;
#7849 = AXIS2_PLACEMENT_3D ( 'NONE', #4396, #1948, #7574 ) ;
#7850 = EDGE_LOOP ( 'NONE', ( #5147, #6558, #2105, #9711 ) ) ;
#7851 = AXIS2_PLACEMENT_3D ( 'NONE', #589, #6306, #7116 ) ;
#7852 = ADVANCED_FACE ( 'NONE', ( #8478 ), #2862, .T. ) ;
#7853 = ORIENTED_EDGE ( 'NONE', *, *, #4427, .F. ) ;
#7854 = ORIENTED_EDGE ( 'NONE', *, *, #4631, .F. ) ;
#7855 = DIRECTION ( 'NONE',  ( -0.000000000000000000, -0.000000000000000000, -1.000000000000000000 ) ) ;
#7856 = DIRECTION ( 'NONE',  ( 1.000000000000000000, -0.000000000000000000, -0.000000000000000000 ) ) ;
#7857 = AXIS2_PLACEMENT_3D ( 'NONE', #4424, #7660, #5117 ) ;
#7858 = LINE ( 'NONE', #657, #452 ) ;
#7859 = DIRECTION ( 'NONE',  ( 0.6691306063588559061, 0.7431448254773963535, 0.000000000000000000 ) ) ;
#7860 = PRODUCT_DEFINITION_FORMATION_WITH_SPECIFIED_SOURCE ( 'ANY', '', #3828, .NOT_KNOWN. ) ;
#7861 = CARTESIAN_POINT ( 'NONE',  ( -23.15769640663937423, -117.1457019118819005, -48.00000000000002132 ) ) ;
#7862 = EDGE_LOOP ( 'NONE', ( #9882, #10162, #1537, #2412 ) ) ;
#7863 = CARTESIAN_POINT ( 'NONE',  ( -2.293506896408097795, 120.5696653505793705, 20.00000000000000711 ) ) ;
#7864 = TOROIDAL_SURFACE ( 'NONE', #2285, 26.75575292317714471, 5.000000000000000000 ) ;
#7865 = ADVANCED_FACE ( 'NONE', ( #3665 ), #6145, .F. ) ;
#7866 = EDGE_CURVE ( 'NONE', #10322, #7089, #10027, .T. ) ;
#7867 = VERTEX_POINT ( 'NONE', #2805 ) ;
#7868 = CARTESIAN_POINT ( 'NONE',  ( -1.071796769724492338, -4.000000000000000000, -4.898587196589413815E-16 ) ) ;
#7869 = CIRCLE ( 'NONE', #3467, 3.297986701801175258 ) ;
#7870 = CARTESIAN_POINT ( 'NONE',  ( -39.00436953563450970, -0.03089877619826558730, 3.555871974361681342 ) ) ;
#7871 = FACE_OUTER_BOUND ( 'NONE', #9211, .T. ) ;
#7872 = CARTESIAN_POINT ( 'NONE',  ( 37.22511195853868315, -116.3672949040187063, 25.00000000000000000 ) ) ;
#7873 = VERTEX_POINT ( 'NONE', #9386 ) ;
#7874 = CIRCLE ( 'NONE', #2452, 3.999999999999996447 ) ;
#7875 = CYLINDRICAL_SURFACE ( 'NONE', #1734, 4.000000000000000000 ) ;
#7876 =( LENGTH_UNIT ( ) NAMED_UNIT ( * ) SI_UNIT ( .MILLI., .METRE. ) );
#7878 = ADVANCED_FACE ( 'NONE', ( #1958 ), #8588, .F. ) ;
#7877 = ORIENTED_EDGE ( 'NONE', *, *, #3926, .F. ) ;
#7879 = EDGE_CURVE ( 'NONE', #4943, #9316, #4953, .T. ) ;
#7880 = DIRECTION ( 'NONE',  ( 0.000000000000000000, 0.000000000000000000, 1.000000000000000000 ) ) ;
#7881 = ORIENTED_EDGE ( 'NONE', *, *, #7928, .T. ) ;
#7882 = APPLICATION_CONTEXT ( 'automotive_design' ) ;
#7883 = EDGE_LOOP ( 'NONE', ( #7631, #6260, #3052, #3357 ) ) ;
#7884 = CARTESIAN_POINT ( 'NONE',  ( -56.36957570605425616, 90.52895752738122326, 10.90000000000000036 ) ) ;
#7885 = PLANE ( 'NONE',  #7152 ) ;
#7886 = FACE_OUTER_BOUND ( 'NONE', #6335, .T. ) ;
#7887 = DIRECTION ( 'NONE',  ( -0.000000000000000000, 1.000000000000000000, -0.000000000000000000 ) ) ;
#7888 = CARTESIAN_POINT ( 'NONE',  ( -27.15769640663940976, -115.1457019118818863, 27.15769640663938489 ) ) ;
#7889 = CIRCLE ( 'NONE', #9414, 20.00000000000000000 ) ;
#7890 = FACE_BOUND ( 'NONE', #2657, .T. ) ;
#7891 = CYLINDRICAL_SURFACE ( 'NONE', #6314, 3.999999999999989786 ) ;
#7892 = PRODUCT ( 'Secondary Joint', 'Secondary Joint', '', ( #8617 ) ) ;
#7893 = VECTOR ( 'NONE', #3267, 1000.000000000000000 ) ;
#7894 = VERTEX_POINT ( 'NONE', #1330 ) ;
#7895 = CARTESIAN_POINT ( 'NONE',  ( -27.15769640663939555, -135.1457019118818721, -27.15769640663944173 ) ) ;
#7896 = AXIS2_PLACEMENT_3D ( 'NONE', #10196, #1971, #2927 ) ;
#7897 = ORIENTED_EDGE ( 'NONE', *, *, #3140, .T. ) ;
#7898 = DIRECTION ( 'NONE',  ( 0.000000000000000000, 0.000000000000000000, 1.000000000000000000 ) ) ;
#7899 = DIRECTION ( 'NONE',  ( 1.000000000000000000, 0.000000000000000000, 0.000000000000000000 ) ) ;
#7900 = AXIS2_PLACEMENT_3D ( 'NONE', #3089, #6104, #7919 ) ;
#7901 = CARTESIAN_POINT ( 'NONE',  ( -16.29350689640809691, -8.660287962196477451, 4.729641367753004033 ) ) ;
#7902 = EDGE_CURVE ( 'NONE', #939, #3699, #9225, .T. ) ;
#7903 = PLANE ( 'NONE',  #2116 ) ;
#7904 = B_SPLINE_CURVE_WITH_KNOTS ( 'NONE', 3,
 ( #1595, #8055, #5516, #4036, #10353, #1499, #3034, #10401, #10453, #2978 ),
 .UNSPECIFIED., .F., .F.,
 ( 4, 2, 2, 2, 4 ),
 ( -8.944271910604867948E-06, 0.001019331502940706933, 0.002047607277792018454, 0.003075883052643329976, 0.004104158827494642364 ),
 .UNSPECIFIED. ) ;
#7905 = DIRECTION ( 'NONE',  ( 0.000000000000000000, 0.000000000000000000, -1.000000000000000000 ) ) ;
#7906 = ORIENTED_EDGE ( 'NONE', *, *, #8580, .T. ) ;
#7907 = VECTOR ( 'NONE', #7203, 1000.000000000000000 ) ;
#7908 = ORIENTED_EDGE ( 'NONE', *, *, #8889, .T. ) ;
#7909 =( GEOMETRIC_REPRESENTATION_CONTEXT ( 3 ) GLOBAL_UNCERTAINTY_ASSIGNED_CONTEXT ( ( #4204 ) ) GLOBAL_UNIT_ASSIGNED_CONTEXT ( ( #520, #3110, #1527 ) ) REPRESENTATION_CONTEXT ( 'NONE', 'WORKASPACE' ) );
#7910 = VERTEX_POINT ( 'NONE', #8375 ) ;
#7911 = ORIENTED_EDGE ( 'NONE', *, *, #731, .T. ) ;
#7912 = FACE_OUTER_BOUND ( 'NONE', #9391, .T. ) ;
#7913 = DIRECTION ( 'NONE',  ( 0.000000000000000000, 0.000000000000000000, 1.000000000000000000 ) ) ;
#7914 = CIRCLE ( 'NONE', #9085, 2.000000000000001776 ) ;
#7915 = DIRECTION ( 'NONE',  ( -1.000000000000000000, 0.000000000000000000, 0.000000000000000000 ) ) ;
#7916 = CARTESIAN_POINT ( 'NONE',  ( -43.93820948810023452, 4.000000000000000888, 0.000000000000000000 ) ) ;
#7917 = VECTOR ( 'NONE', #9409, 1000.000000000000000 ) ;
#7918 = ADVANCED_FACE ( 'NONE', ( #2065 ), #728, .T. ) ;
#7919 = DIRECTION ( 'NONE',  ( 0.000000000000000000, -0.000000000000000000, -1.000000000000000000 ) ) ;
#7920 = ORIENTED_EDGE ( 'NONE', *, *, #5288, .T. ) ;
#7921 = LINE ( 'NONE', #3899, #9170 ) ;
#7922 = CONICAL_SURFACE ( 'NONE', #3351, 2.445500000000000007, 0.7853981633974547183 ) ;
#7923 = ORIENTED_EDGE ( 'NONE', *, *, #4357, .F. ) ;
#7924 = DIRECTION ( 'NONE',  ( 0.000000000000000000, 1.000000000000000000, 0.000000000000000000 ) ) ;
#7925 = VECTOR ( 'NONE', #1342, 1000.000000000000000 ) ;
#7926 = LINE ( 'NONE', #6274, #1480 ) ;
#7927 =( BOUNDED_CURVE ( )  B_SPLINE_CURVE ( 3, ( #6632, #4299, #4247, #8629 ),
 .UNSPECIFIED., .F., .F. ) 
 B_SPLINE_CURVE_WITH_KNOTS ( ( 4, 4 ),
 ( 5.245636577995398397, 5.314071712302153472 ),
 .UNSPECIFIED. ) 
 CURVE ( )  GEOMETRIC_REPRESENTATION_ITEM ( )  RATIONAL_B_SPLINE_CURVE ( ( 1.000000000000000000, 0.9996097574442918132, 0.9996097574442918132, 1.000000000000000000 ) ) 
 REPRESENTATION_ITEM ( '' )  );
#7928 = EDGE_CURVE ( 'NONE', #4096, #5226, #331, .T. ) ;
#7929 = FACE_OUTER_BOUND ( 'NONE', #6262, .T. ) ;
#7930 = VERTEX_POINT ( 'NONE', #482 ) ;
#7931 = CARTESIAN_POINT ( 'NONE',  ( 25.44550000000000978, 3.673940397442059868E-16, -2.999999999999999556 ) ) ;
#7932 = ORIENTED_EDGE ( 'NONE', *, *, #8199, .F. ) ;
#7933 = CIRCLE ( 'NONE', #3365, 6.499999999999964473 ) ;
#7934 = DIRECTION ( 'NONE',  ( -0.6691306063588560171, -0.7431448254773961315, 0.000000000000000000 ) ) ;
#7935 = VERTEX_POINT ( 'NONE', #1115 ) ;
#7936 = AXIS2_PLACEMENT_3D ( 'NONE', #5545, #4739, #7934 ) ;
#7937 = ORIENTED_EDGE ( 'NONE', *, *, #4742, .T. ) ;
#7938 = CARTESIAN_POINT ( 'NONE',  ( -30.29350689640809335, 55.56966535057937051, 0.000000000000000000 ) ) ;
#7939 = DIRECTION ( 'NONE',  ( 1.000000000000000000, 0.000000000000000000, 8.379529552680124346E-16 ) ) ;
#7940 = DIRECTION ( 'NONE',  ( -1.000000000000000000, 0.000000000000000000, 0.000000000000000000 ) ) ;
#7941 = ADVANCED_FACE ( 'NONE', ( #10183, #532 ), #5984, .F. ) ;
#7942 = EDGE_CURVE ( 'NONE', #8369, #4089, #10044, .T. ) ;
#7943 = CARTESIAN_POINT ( 'NONE',  ( -30.29350689640809335, 80.56966535057935630, -20.00000000000000711 ) ) ;
#7944 = EDGE_CURVE ( 'NONE', #939, #9477, #7325, .T. ) ;
#7945 = LINE ( 'NONE', #5553, #4245 ) ;
#7946 = VECTOR ( 'NONE', #3372, 1000.000000000000000 ) ;
#7947 = ORIENTED_EDGE ( 'NONE', *, *, #4771, .F. ) ;
#7948 = DIRECTION ( 'NONE',  ( 0.000000000000000000, 0.000000000000000000, 1.000000000000000000 ) ) ;
#7949 = VERTEX_POINT ( 'NONE', #7634 ) ;
#7950 = DIRECTION ( 'NONE',  ( 1.000000000000000000, 0.000000000000000000, -2.154935995002246132E-16 ) ) ;
#7951 = DIRECTION ( 'NONE',  ( 1.000000000000000000, -0.000000000000000000, -0.000000000000000000 ) ) ;
#7952 = ORIENTED_EDGE ( 'NONE', *, *, #3992, .T. ) ;
#7953 = VECTOR ( 'NONE', #8308, 1000.000000000000000 ) ;
#7954 = CARTESIAN_POINT ( 'NONE',  ( -16.29350689640809691, 11.33971203780352255, 0.000000000000000000 ) ) ;
#7955 = FACE_OUTER_BOUND ( 'NONE', #9820, .T. ) ;
#7956 = EDGE_CURVE ( 'NONE', #6390, #6245, #3102, .T. ) ;
#7957 = DIRECTION ( 'NONE',  ( 1.000000000000000000, 0.000000000000000000, 0.000000000000000000 ) ) ;
#7958 = ORIENTED_EDGE ( 'NONE', *, *, #500, .F. ) ;
#7959 = VERTEX_POINT ( 'NONE', #4457 ) ;
#7960 = ORIENTED_EDGE ( 'NONE', *, *, #4501, .F. ) ;
#7961 = PLANE ( 'NONE',  #9102 ) ;
#7962 = CARTESIAN_POINT ( 'NONE',  ( -23.15769640663937423, -133.1457019118818721, -48.00000000000002132 ) ) ;
#7963 = DIRECTION ( 'NONE',  ( 9.776117811460147207E-16, -0.000000000000000000, -1.000000000000000000 ) ) ;
#7964 = PLANE ( 'NONE',  #4945 ) ;
#7965 = CARTESIAN_POINT ( 'NONE',  ( -2.293506896408097795, 150.5696653505793563, 0.000000000000000000 ) ) ;
#7966 = ORIENTED_EDGE ( 'NONE', *, *, #8084, .T. ) ;
#7967 = DIRECTION ( 'NONE',  ( -1.000000000000000000, 0.000000000000000000, 0.000000000000000000 ) ) ;
#7968 = ADVANCED_FACE ( 'NONE', ( #10079 ), #7690, .F. ) ;
#7969 = ORIENTED_EDGE ( 'NONE', *, *, #5714, .F. ) ;
#7970 = AXIS2_PLACEMENT_3D ( 'NONE', #7679, #5286, #2006 ) ;
#7971 = CARTESIAN_POINT ( 'NONE',  ( -25.15769640663940265, -115.1457019118818863, -3.513494341946491635E-15 ) ) ;
#7972 = B_SPLINE_CURVE_WITH_KNOTS ( 'NONE', 3,
 ( #3134, #9667, #6212, #8008, #2386, #5620, #3893, #2294, #9454, #5415 ),
 .UNSPECIFIED., .F., .F.,
 ( 4, 2, 2, 2, 4 ),
 ( 0.000000000000000000, 0.001023740819106960624, 0.002047481638213921248, 0.003071222457320881873, 0.004094963276427842497 ),
 .UNSPECIFIED. ) ;
#7973 = CARTESIAN_POINT ( 'NONE',  ( 26.27514770175546843, -135.1457019118818721, -50.00000000000001421 ) ) ;
#7974 = CARTESIAN_POINT ( 'NONE',  ( -16.29350689640809691, 76.32362273389503571, 0.000000000000000000 ) ) ;
#7975 = ORIENTED_EDGE ( 'NONE', *, *, #805, .T. ) ;
#7976 = AXIS2_PLACEMENT_3D ( 'NONE', #5996, #1234, #4467 ) ;
#7977 = CARTESIAN_POINT ( 'NONE',  ( -47.94539818030330025, 150.5696653505793563, -3.999999999999993339 ) ) ;
#7978 =( NAMED_UNIT ( * ) PLANE_ANGLE_UNIT ( ) SI_UNIT ( $, .RADIAN. ) );
#7979 = ORIENTED_EDGE ( 'NONE', *, *, #9637, .T. ) ;
#7980 = DIRECTION ( 'NONE',  ( -1.000000000000000000, 0.000000000000000000, 0.000000000000000000 ) ) ;
#7981 = EDGE_CURVE ( 'NONE', #9529, #2212, #8690, .T. ) ;
#7982 = ORIENTED_EDGE ( 'NONE', *, *, #7347, .T. ) ;
#7983 = AXIS2_PLACEMENT_3D ( 'NONE', #1991, #3582, #2887 ) ;
#7984 = CARTESIAN_POINT ( 'NONE',  ( -39.00428932080996702, 3.095342794014916965, -1.752073144804183080 ) ) ;
#7985 = CARTESIAN_POINT ( 'NONE',  ( 53.40242741783141156, 147.5696653505793279, 25.00000000000000000 ) ) ;
#7986 = FACE_OUTER_BOUND ( 'NONE', #8312, .T. ) ;
#7987 = CYLINDRICAL_SURFACE ( 'NONE', #7137, 4.024999999999997691 ) ;
#7988 = PLANE ( 'NONE',  #9079 ) ;
#7989 = VECTOR ( 'NONE', #3518, 1000.000000000000000 ) ;
#7990 = ORIENTED_EDGE ( 'NONE', *, *, #1669, .T. ) ;
#7991 = CARTESIAN_POINT ( 'NONE',  ( -7.293506896408097795, 0.000000000000000000, 0.000000000000000000 ) ) ;
#7992 = ADVANCED_FACE ( 'NONE', ( #7261 ), #6321, .F. ) ;
#7993 = EDGE_CURVE ( 'NONE', #898, #869, #5457, .T. ) ;
#7994 = EDGE_CURVE ( 'NONE', #1439, #4025, #3124, .T. ) ;
#7995 = EDGE_LOOP ( 'NONE', ( #3912, #6914 ) ) ;
#7996 = CARTESIAN_POINT ( 'NONE',  ( 37.22511195853868315, -116.3672949040186779, -25.00000000000000355 ) ) ;
#7997 = CIRCLE ( 'NONE', #6313, 1.999999999999998224 ) ;
#7998 = AXIS2_PLACEMENT_3D ( 'NONE', #7298, #7458, #202 ) ;
#7999 = CARTESIAN_POINT ( 'NONE',  ( 37.22511195853869026, -145.1457019118819005, -30.00000000000000355 ) ) ;
#8000 = DIRECTION ( 'NONE',  ( -0.000000000000000000, -1.000000000000000000, -0.000000000000000000 ) ) ;
#8001 = LINE ( 'NONE', #5612, #9577 ) ;
#8002 = EDGE_LOOP ( 'NONE', ( #8301, #1524, #4485, #6686 ) ) ;
#8003 = ORIENTED_EDGE ( 'NONE', *, *, #1177, .F. ) ;
#8004 = AXIS2_PLACEMENT_3D ( 'NONE', #8276, #3447, #7477 ) ;
#8005 = VERTEX_POINT ( 'NONE', #2377 ) ;
#8006 = ADVANCED_FACE ( 'NONE', ( #3176 ), #1067, .F. ) ;
#8007 = DIRECTION ( 'NONE',  ( 0.000000000000000000, 0.000000000000000000, 1.000000000000000000 ) ) ;
#8008 = CARTESIAN_POINT ( 'NONE',  ( 25.28852788137212926, -134.8487249201535008, 49.99999999999997868 ) ) ;
#8009 = DIRECTION ( 'NONE',  ( 1.000000000000000000, 0.000000000000000000, 6.982941293900105430E-16 ) ) ;
#8010 = CARTESIAN_POINT ( 'NONE',  ( 3.000000000000000000, 1.467624384280032501, 2.541999999999999371 ) ) ;
#8011 = VECTOR ( 'NONE', #946, 1000.000000000000114 ) ;
#8012 = DIRECTION ( 'NONE',  ( -0.7431448254773957984, 0.6691306063588565722, -0.000000000000000000 ) ) ;
#8013 = ORIENTED_EDGE ( 'NONE', *, *, #10202, .T. ) ;
#8014 = DIRECTION ( 'NONE',  ( -6.964995403156261684E-17, -0.08715574274766944851, 0.9961946980917446570 ) ) ;
#8015 = AXIS2_PLACEMENT_3D ( 'NONE', #4381, #3693, #6809 ) ;
#8016 = ORIENTED_EDGE ( 'NONE', *, *, #2562, .T. ) ;
#8017 = DIRECTION ( 'NONE',  ( -1.000000000000000000, -0.000000000000000000, -0.000000000000000000 ) ) ;
#8018 = PRODUCT_DEFINITION_FORMATION_WITH_SPECIFIED_SOURCE ( 'ANY', '', #2307, .NOT_KNOWN. ) ;
#8019 = CARTESIAN_POINT ( 'NONE',  ( 59.99999999999997868, -145.1457019118819005, 30.00000000000000355 ) ) ;
#8020 = ADVANCED_FACE ( 'NONE', ( #6456, #692 ), #4808, .F. ) ;
#8021 = CARTESIAN_POINT ( 'NONE',  ( 37.39675911933730390, -134.9593434439503312, -26.30486341150395901 ) ) ;
#8022 = CIRCLE ( 'NONE', #10411, 3.297986701801175258 ) ;
#8023 = ORIENTED_EDGE ( 'NONE', *, *, #80, .T. ) ;
#8024 = DIRECTION ( 'NONE',  ( 0.000000000000000000, 0.000000000000000000, -1.000000000000000000 ) ) ;
#8025 = TOROIDAL_SURFACE ( 'NONE', #594, 16.62298474266377468, 9.050254677131421843 ) ;
#8026 = ITEM_DEFINED_TRANSFORMATION ( 'NONE', 'NONE', #4962,  #4601 ) ;
#8027 = ORIENTED_EDGE ( 'NONE', *, *, #7674, .T. ) ;
#8028 = CARTESIAN_POINT ( 'NONE',  ( 6.756858349438872757, 146.7073643690755773, 30.00000000000000355 ) ) ;
#8029 = ORIENTED_EDGE ( 'NONE', *, *, #2562, .F. ) ;
#8030 = CIRCLE ( 'NONE', #1941, 31.75575292317714471 ) ;
#8031 = CYLINDRICAL_SURFACE ( 'NONE', #8754, 7.500000000000000000 ) ;
#8032 = AXIS2_PLACEMENT_3D ( 'NONE', #9759, #6511, #7519 ) ;
#8033 = DIRECTION ( 'NONE',  ( -0.000000000000000000, 1.000000000000000000, -0.000000000000000000 ) ) ;
#8034 = CARTESIAN_POINT ( 'NONE',  ( 27.15769640663938489, -135.1457019118818721, -27.15769640663940976 ) ) ;
#8035 = FACE_BOUND ( 'NONE', #6602, .T. ) ;
#8036 = DIRECTION ( 'NONE',  ( 0.000000000000000000, 0.000000000000000000, -1.000000000000000000 ) ) ;
#8037 = ADVANCED_FACE ( 'NONE', ( #9608 ), #2177, .F. ) ;
#8038 = EDGE_LOOP ( 'NONE', ( #2613, #6952 ) ) ;
#8039 = AXIS2_PLACEMENT_3D ( 'NONE', #4548, #10124, #2851 ) ;
#8040 = CARTESIAN_POINT ( 'NONE',  ( -16.29350689640809691, 37.08684478514406635, 7.500000000000000000 ) ) ;
#8041 = ORIENTED_EDGE ( 'NONE', *, *, #2762, .T. ) ;
#8042 = DIRECTION ( 'NONE',  ( -0.000000000000000000, -0.000000000000000000, 1.000000000000000000 ) ) ;
#8043 = LINE ( 'NONE', #5019, #3082 ) ;
#8044 = DIRECTION ( 'NONE',  ( 1.000000000000000000, -0.000000000000000000, -0.000000000000000000 ) ) ;
#8045 = DIRECTION ( 'NONE',  ( 0.000000000000000000, 0.000000000000000000, 1.000000000000000000 ) ) ;
#8046 = VECTOR ( 'NONE', #9045, 999.9999999999998863 ) ;
#8047 = FACE_OUTER_BOUND ( 'NONE', #6903, .T. ) ;
#8048 = VERTEX_POINT ( 'NONE', #5506 ) ;
#8049 = EDGE_CURVE ( 'NONE', #1443, #9987, #5608, .T. ) ;
#8050 = EDGE_CURVE ( 'NONE', #9059, #8005, #788, .T. ) ;
#8051 = VECTOR ( 'NONE', #918, 1000.000000000000000 ) ;
#8052 = PRODUCT ( 'socket head cap screw_iso_ISO 4762 M6 x 20 - 20N', 'socket head cap screw_iso_ISO 4762 M6 x 20 - 20N', '', ( #6979 ) ) ;
#8053 = CIRCLE ( 'NONE', #5182, 4.000000000000000000 ) ;
#8054 = VERTEX_POINT ( 'NONE', #3025 ) ;
#8055 = CARTESIAN_POINT ( 'NONE',  ( -50.00000000000001421, -133.3880685334790144, -23.40006363392675937 ) ) ;
#8056 = CARTESIAN_POINT ( 'NONE',  ( -39.65557114539780770, -0.1824758893689537032, 3.996877754856925424 ) ) ;
#8057 = DIRECTION ( 'NONE',  ( 0.000000000000000000, -1.222897680782651471E-16, 1.000000000000000000 ) ) ;
#8058 = CARTESIAN_POINT ( 'NONE',  ( -11.56386552865509110, 65.65569765742554864, 0.000000000000000000 ) ) ;
#8059 = AXIS2_PLACEMENT_3D ( 'NONE', #3763, #9382, #4500 ) ;
#8060 = EDGE_LOOP ( 'NONE', ( #9116, #7952, #1940 ) ) ;
#8061 = EDGE_CURVE ( 'NONE', #2182, #826, #3224, .T. ) ;
#8062 = DIRECTION ( 'NONE',  ( 0.000000000000000000, -1.000000000000000000, 1.222897680782651224E-16 ) ) ;
#8063 = EDGE_CURVE ( 'NONE', #2146, #4613, #9712, .T. ) ;
#8064 = AXIS2_PLACEMENT_3D ( 'NONE', #8381, #8278, #6738 ) ;
#8065 = ADVANCED_FACE ( 'NONE', ( #643 ), #4759, .F. ) ;
#8066 = ORIENTED_EDGE ( 'NONE', *, *, #994, .T. ) ;
#8067 = FACE_OUTER_BOUND ( 'NONE', #3184, .T. ) ;
#8068 = AXIS2_PLACEMENT_3D ( 'NONE', #7991, #1682, #7948 ) ;
#8069 = ORIENTED_EDGE ( 'NONE', *, *, #8641, .T. ) ;
#8070 = VERTEX_POINT ( 'NONE', #7845 ) ;
#8071 = DIRECTION ( 'NONE',  ( 0.000000000000000000, 0.000000000000000000, 1.000000000000000000 ) ) ;
#8072 = AXIS2_PLACEMENT_3D ( 'NONE', #6495, #9741, #2632 ) ;
#8073 = DIRECTION ( 'NONE',  ( -0.000000000000000000, -0.000000000000000000, -1.000000000000000000 ) ) ;
#8074 = DIRECTION ( 'NONE',  ( 1.137729606058012035E-16, 0.000000000000000000, 1.000000000000000000 ) ) ;
#8075 = DIRECTION ( 'NONE',  ( 1.000000000000000000, 0.000000000000000000, 0.000000000000000000 ) ) ;
#8076 = AXIS2_PLACEMENT_3D ( 'NONE', #505, #3737, #6968 ) ;
#8077 = EDGE_CURVE ( 'NONE', #2596, #2698, #3882, .T. ) ;
#8078 = VERTEX_POINT ( 'NONE', #588 ) ;
#8079 = DIRECTION ( 'NONE',  ( -1.000000000000000000, 0.000000000000000000, 0.000000000000000000 ) ) ;
#8080 = AXIS2_PLACEMENT_3D ( 'NONE', #8966, #5139, #6736 ) ;
#8081 = EDGE_LOOP ( 'NONE', ( #9997, #3004, #2844, #8451, #2816 ) ) ;
#8082 = CARTESIAN_POINT ( 'NONE',  ( -16.29350689640809691, 76.32362273389503571, -4.729641367753004033 ) ) ;
#8083 = EDGE_LOOP ( 'NONE', ( #9818, #1510 ) ) ;
#8084 = EDGE_CURVE ( 'NONE', #6283, #2948, #4624, .T. ) ;
#8085 = ORIENTED_EDGE ( 'NONE', *, *, #4463, .T. ) ;
#8086 = CARTESIAN_POINT ( 'NONE',  ( -56.36957570605427037, 137.0132282531173473, 0.000000000000000000 ) ) ;
#8087 = DIRECTION ( 'NONE',  ( -1.000000000000000000, 0.000000000000000000, 0.000000000000000000 ) ) ;
#8088 = DIRECTION ( 'NONE',  ( 0.000000000000000000, -1.222897680782651471E-16, 1.000000000000000000 ) ) ;
#8089 = LINE ( 'NONE', #1679, #8304 ) ;
#8090 = CARTESIAN_POINT ( 'NONE',  ( 99.80027788547053547, -145.1457019118819005, -27.92893218813452094 ) ) ;
#8091 = AXIS2_PLACEMENT_3D ( 'NONE', #7055, #10291, #1433 ) ;
#8092 = ORIENTED_EDGE ( 'NONE', *, *, #4942, .T. ) ;
#8093 = PLANE ( 'NONE',  #8068 ) ;
#8094 = AXIS2_PLACEMENT_3D ( 'NONE', #10374, #9586, #4699 ) ;
#8095 = VERTEX_POINT ( 'NONE', #4028 ) ;
#8096 = CARTESIAN_POINT ( 'NONE',  ( -24.29350689640808625, 140.5696653505793563, 20.00000000000002132 ) ) ;
#8097 = DIRECTION ( 'NONE',  ( 1.000000000000000000, 0.000000000000000000, 1.396588258780020149E-16 ) ) ;
#8098 = SURFACE_SIDE_STYLE ('',( #9704 ) ) ;
#8099 = LINE ( 'NONE', #163, #3957 ) ;
#8100 = LINE ( 'NONE', #7310, #1446 ) ;
#8101 = CARTESIAN_POINT ( 'NONE',  ( 77.30044127146538813, 73.68369600860394542, -12.50000000000000000 ) ) ;
#8102 = CIRCLE ( 'NONE', #8611, 4.000000000000000000 ) ;
#8103 = ORIENTED_EDGE ( 'NONE', *, *, #3524, .F. ) ;
#8104 = ADVANCED_FACE ( 'NONE', ( #7115 ), #3071, .F. ) ;
#8105 = ORIENTED_EDGE ( 'NONE', *, *, #7032, .F. ) ;
#8106 = ORIENTED_EDGE ( 'NONE', *, *, #8061, .T. ) ;
#8107 = ORIENTED_EDGE ( 'NONE', *, *, #3867, .F. ) ;
#8108 = PRESENTATION_LAYER_ASSIGNMENT (  '', '', ( #3380 ) ) ;
#8109 = EDGE_CURVE ( 'NONE', #3359, #5589, #4073, .T. ) ;
#8110 = DIRECTION ( 'NONE',  ( 0.000000000000000000, 0.000000000000000000, 1.000000000000000000 ) ) ;
#8111 = FILL_AREA_STYLE ('',( #9771 ) ) ;
#8112 = DIRECTION ( 'NONE',  ( 0.000000000000000000, 0.000000000000000000, 1.000000000000000000 ) ) ;
#8113 = DIRECTION ( 'NONE',  ( -1.000000000000000000, -0.000000000000000000, -0.000000000000000000 ) ) ;
#8114 = VERTEX_POINT ( 'NONE', #4183 ) ;
#8115 = PLANE ( 'NONE',  #9936 ) ;
#8116 = ORIENTED_EDGE ( 'NONE', *, *, #5096, .F. ) ;
#8117 = CARTESIAN_POINT ( 'NONE',  ( -2.293506896408097795, 37.08684478514406635, -24.99999999999998934 ) ) ;
#8118 = ORIENTED_EDGE ( 'NONE', *, *, #1262, .F. ) ;
#8119 = EDGE_CURVE ( 'NONE', #5197, #4096, #6670, .T. ) ;
#8120 = PLANE ( 'NONE',  #4701 ) ;
#8121 = EDGE_CURVE ( 'NONE', #4224, #5528, #9812, .T. ) ;
#8122 = DIRECTION ( 'NONE',  ( 0.000000000000000000, 0.000000000000000000, -1.000000000000000000 ) ) ;
#8123 = EDGE_CURVE ( 'NONE', #4400, #9740, #8099, .T. ) ;
#8124 = CARTESIAN_POINT ( 'NONE',  ( -30.29350689640809335, 2.445795361565304815E-15, -20.00000000000002132 ) ) ;
#8125 = DIRECTION ( 'NONE',  ( 1.000000000000000000, -8.585830317548973933E-16, 0.000000000000000000 ) ) ;
#8126 = CARTESIAN_POINT ( 'NONE',  ( -20.29350689640809691, 140.5696653505793563, 10.90000000000000036 ) ) ;
#8127 = ORIENTED_EDGE ( 'NONE', *, *, #9639, .T. ) ;
#8128 = FACE_OUTER_BOUND ( 'NONE', #1030, .T. ) ;
#8129 = CONTEXT_DEPENDENT_SHAPE_REPRESENTATION ( #1661, #5512 ) ;
#8130 = ORIENTED_EDGE ( 'NONE', *, *, #5069, .F. ) ;
#8131 = CARTESIAN_POINT ( 'NONE',  ( -8.000000000000000000, 1.691446717414637479, 1.184363742013802900 ) ) ;
#8132 = EDGE_LOOP ( 'NONE', ( #2156, #794, #4410, #6750 ) ) ;
#8133 = EDGE_CURVE ( 'NONE', #9263, #1359, #8309, .T. ) ;
#8134 = CARTESIAN_POINT ( 'NONE',  ( -30.29350689640809335, 120.5696653505793705, -20.00000000000000711 ) ) ;
#8135 = AXIS2_PLACEMENT_3D ( 'NONE', #8471, #10067, #2795 ) ;
#8136 = DIRECTION ( 'NONE',  ( -1.000000000000000000, -0.000000000000000000, 0.000000000000000000 ) ) ;
#8137 = FACE_OUTER_BOUND ( 'NONE', #6329, .T. ) ;
#8138 = DIRECTION ( 'NONE',  ( 0.000000000000000000, 0.000000000000000000, -1.000000000000000000 ) ) ;
#8139 = FACE_OUTER_BOUND ( 'NONE', #5300, .T. ) ;
#8140 = EDGE_LOOP ( 'NONE', ( #8596, #7760, #2837, #111 ) ) ;
#8141 = AXIS2_PLACEMENT_3D ( 'NONE', #5213, #348, #5312 ) ;
#8142 = DIRECTION ( 'NONE',  ( -0.7431448254773957984, 0.6691306063588565722, -0.000000000000000000 ) ) ;
#8143 = AXIS2_PLACEMENT_3D ( 'NONE', #9254, #358, #5959 ) ;
#8144 = VERTEX_POINT ( 'NONE', #9865 ) ;
#8145 = DIRECTION ( 'NONE',  ( -0.6691306063588547959, -0.7431448254773973527, 0.000000000000000000 ) ) ;
#8146 = DIRECTION ( 'NONE',  ( 1.000000000000000000, 0.000000000000000000, 0.000000000000000000 ) ) ;
#8147 = DIRECTION ( 'NONE',  ( 0.000000000000000000, -0.000000000000000000, -1.000000000000000000 ) ) ;
#8148 = CARTESIAN_POINT ( 'NONE',  ( 14.70649310359190309, 80.56966535057935630, -16.00000000000000711 ) ) ;
#8149 = CARTESIAN_POINT ( 'NONE',  ( -149.7944168144651655, 241.1335534508485807, 0.000000000000000000 ) ) ;
#8150 = AXIS2_PLACEMENT_3D ( 'NONE', #10313, #4683, #8764 ) ;
#8151 = APPLICATION_CONTEXT ( 'automotive_design' ) ;
#8152 = DIRECTION ( 'NONE',  ( -0.000000000000000000, 1.000000000000000000, 0.000000000000000000 ) ) ;
#8153 = AXIS2_PLACEMENT_3D ( 'NONE', #1274, #1169, #6948 ) ;
#8154 = ORIENTED_EDGE ( 'NONE', *, *, #4930, .F. ) ;
#8155 = EDGE_CURVE ( 'NONE', #6555, #4407, #7340, .T. ) ;
#8156 = ORIENTED_EDGE ( 'NONE', *, *, #8258, .F. ) ;
#8157 = ORIENTED_EDGE ( 'NONE', *, *, #7538, .F. ) ;
#8158 = CONICAL_SURFACE ( 'NONE', #6463, 4.025000000000000355, 0.7853981633973787790 ) ;
#8159 = EDGE_LOOP ( 'NONE', ( #6221, #4913, #873, #6281 ) ) ;
#8160 = AXIS2_PLACEMENT_3D ( 'NONE', #5539, #563, #2358 ) ;
#8161 = DIRECTION ( 'NONE',  ( -1.000000000000000000, -0.000000000000000000, -0.000000000000000000 ) ) ;
#8162 = DIRECTION ( 'NONE',  ( -0.000000000000000000, 1.000000000000000000, -0.000000000000000000 ) ) ;
#8163 = DIRECTION ( 'NONE',  ( 0.000000000000000000, 0.000000000000000000, 1.000000000000000000 ) ) ;
#8164 = DIRECTION ( 'NONE',  ( 1.000000000000000000, -0.000000000000000000, -0.000000000000000000 ) ) ;
#8165 = ORIENTED_EDGE ( 'NONE', *, *, #9849, .T. ) ;
#8166 = CARTESIAN_POINT ( 'NONE',  ( -2.293506896408097795, 120.5696653505793705, 24.00000000000000711 ) ) ;
#8167 = VECTOR ( 'NONE', #7493, 1000.000000000000000 ) ;
#8168 = VERTEX_POINT ( 'NONE', #3387 ) ;
#8169 = CIRCLE ( 'NONE', #1058, 10.00000000000000178 ) ;
#8170 = DIRECTION ( 'NONE',  ( -0.7431448254773957984, 0.6691306063588565722, 0.000000000000000000 ) ) ;
#8171 = EDGE_CURVE ( 'NONE', #9480, #10023, #7518, .T. ) ;
#8172 = ORIENTED_EDGE ( 'NONE', *, *, #9829, .F. ) ;
#8173 = ORIENTED_EDGE ( 'NONE', *, *, #3139, .F. ) ;
#8174 = DIRECTION ( 'NONE',  ( -0.000000000000000000, -0.000000000000000000, -1.000000000000000000 ) ) ;
#8175 = FACE_OUTER_BOUND ( 'NONE', #7550, .T. ) ;
#8176 = AXIS2_PLACEMENT_3D ( 'NONE', #6895, #2015, #2119 ) ;
#8177 = CARTESIAN_POINT ( 'NONE',  ( 59.99999999999999289, 52.77167129626698028, -30.00000000000000355 ) ) ;
#8178 = DIRECTION ( 'NONE',  ( -0.7367503238654704578, -0.6761648913424330720, 0.000000000000000000 ) ) ;
#8179 = DIRECTION ( 'NONE',  ( 0.000000000000000000, 0.000000000000000000, -1.000000000000000000 ) ) ;
#8180 = DIRECTION ( 'NONE',  ( 0.000000000000000000, 0.000000000000000000, 1.000000000000000000 ) ) ;
#8181 = ORIENTED_EDGE ( 'NONE', *, *, #2371, .T. ) ;
#8182 = CARTESIAN_POINT ( 'NONE',  ( 85.07264007511442117, 55.10093597859600578, -24.99999999999998934 ) ) ;
#8183 = EDGE_CURVE ( 'NONE', #1994, #1386, #1583, .T. ) ;
#8184 = CIRCLE ( 'NONE', #406, 3.297986701801175258 ) ;
#8185 = EDGE_CURVE ( 'NONE', #2154, #8341, #5811, .T. ) ;
#8186 = EDGE_CURVE ( 'NONE', #3393, #6231, #68, .T. ) ;
#8187 = CONTEXT_DEPENDENT_SHAPE_REPRESENTATION ( #7083, #8907 ) ;
#8188 = ORIENTED_EDGE ( 'NONE', *, *, #302, .T. ) ;
#8189 = DIRECTION ( 'NONE',  ( -1.000000000000000000, -0.000000000000000000, -0.000000000000000000 ) ) ;
#8190 = ORIENTED_EDGE ( 'NONE', *, *, #1584, .T. ) ;
#8191 = AXIS2_PLACEMENT_3D ( 'NONE', #41, #8087, #9743 ) ;
#8192 = DIRECTION ( 'NONE',  ( -0.000000000000000000, 1.000000000000000000, -0.000000000000000000 ) ) ;
#8193 = CARTESIAN_POINT ( 'NONE',  ( -7.293506896408097795, 128.5696653505793847, 20.00000000000000711 ) ) ;
#8194 = CARTESIAN_POINT ( 'NONE',  ( -16.29350689640809691, -8.660287962196477451, -6.499999999999964473 ) ) ;
#8195 = CARTESIAN_POINT ( 'NONE',  ( 6.000000000000005329, 0.000000000000000000, 0.000000000000000000 ) ) ;
#8196 = DIRECTION ( 'NONE',  ( -1.000000000000000000, -0.000000000000000000, -0.000000000000000000 ) ) ;
#8197 = PRODUCT_DEFINITION ( 'UNKNOWN', '', #3452, #914 ) ;
#8198 = EDGE_CURVE ( 'NONE', #8054, #4361, #1637, .T. ) ;
#8199 = EDGE_CURVE ( 'NONE', #3747, #1722, #1047, .T. ) ;
#8200 = ORIENTED_EDGE ( 'NONE', *, *, #6202, .T. ) ;
#8201 = CIRCLE ( 'NONE', #5148, 2.000000000000001776 ) ;
#8202 = DIRECTION ( 'NONE',  ( 1.000000000000000000, 0.000000000000000000, 0.000000000000000000 ) ) ;
#8203 = ORIENTED_EDGE ( 'NONE', *, *, #128, .F. ) ;
#8204 = LINE ( 'NONE', #837, #7259 ) ;
#8205 = FACE_OUTER_BOUND ( 'NONE', #8749, .T. ) ;
#8206 = ORIENTED_EDGE ( 'NONE', *, *, #3868, .T. ) ;
#8207 = DIRECTION ( 'NONE',  ( 0.000000000000000000, 0.000000000000000000, 1.000000000000000000 ) ) ;
#8208 = DIRECTION ( 'NONE',  ( 1.000000000000000000, 0.000000000000000000, 0.000000000000000000 ) ) ;
#8209 = FACE_OUTER_BOUND ( 'NONE', #9937, .T. ) ;
#8210 = VECTOR ( 'NONE', #7957, 1000.000000000000000 ) ;
#8211 = DIRECTION ( 'NONE',  ( 1.000000000000000000, 0.000000000000000000, 0.000000000000000000 ) ) ;
#8212 = AXIS2_PLACEMENT_3D ( 'NONE', #9484, #8627, #7833 ) ;
#8213 = ORIENTED_EDGE ( 'NONE', *, *, #8109, .F. ) ;
#8214 = ORIENTED_EDGE ( 'NONE', *, *, #8317, .T. ) ;
#8215 = ORIENTED_EDGE ( 'NONE', *, *, #5833, .T. ) ;
#8216 = DIRECTION ( 'NONE',  ( -1.000000000000000000, 0.000000000000000000, 0.000000000000000000 ) ) ;
#8217 = ADVANCED_FACE ( 'NONE', ( #2480 ), #3490, .F. ) ;
#8218 = CIRCLE ( 'NONE', #2638, 7.999999999999996447 ) ;
#8219 = APPLICATION_CONTEXT ( 'automotive_design' ) ;
#8220 = DIRECTION ( 'NONE',  ( -1.000000000000000000, -0.000000000000000000, -0.000000000000000000 ) ) ;
#8221 = DIRECTION ( 'NONE',  ( -0.7431448254773956874, 0.6691306063588564612, -0.000000000000000000 ) ) ;
#8222 = ORIENTED_EDGE ( 'NONE', *, *, #5767, .T. ) ;
#8223 = DIRECTION ( 'NONE',  ( 0.07334937666141774781, -0.9973063064792991872, 2.035854170285226689E-16 ) ) ;
#8224 = CIRCLE ( 'NONE', #4000, 5.000000000000004441 ) ;
#8225 = ORIENTED_EDGE ( 'NONE', *, *, #4311, .F. ) ;
#8226 = VECTOR ( 'NONE', #9719, 1000.000000000000114 ) ;
#8227 = EDGE_LOOP ( 'NONE', ( #7431, #349, #6610, #8003, #8269, #6384 ) ) ;
#8228 = PRODUCT_DEFINITION_CONTEXT ( 'detailed design', #4085, 'design' ) ;
#8229 = CARTESIAN_POINT ( 'NONE',  ( -20.29350689640809691, 140.5696653505793563, -20.00000000000000711 ) ) ;
#8230 = CYLINDRICAL_SURFACE ( 'NONE', #376, 4.000000000000000000 ) ;
#8231 = CIRCLE ( 'NONE', #5856, 7.999999999999996447 ) ;
#8232 = DIRECTION ( 'NONE',  ( 0.08084652178105140863, 0.4212348471733803335, -0.9033410449230815376 ) ) ;
#8233 = LINE ( 'NONE', #1820, #2253 ) ;
#8234 = AXIS2_PLACEMENT_3D ( 'NONE', #1346, #7807, #548 ) ;
#8235 = DIRECTION ( 'NONE',  ( -0.000000000000000000, -0.000000000000000000, -1.000000000000000000 ) ) ;
#8236 = FACE_BOUND ( 'NONE', #5377, .T. ) ;
#8237 = ORIENTED_EDGE ( 'NONE', *, *, #9537, .T. ) ;
#8238 = LINE ( 'NONE', #1614, #4948 ) ;
#8239 = VECTOR ( 'NONE', #7825, 1000.000000000000000 ) ;
#8240 = ORIENTED_EDGE ( 'NONE', *, *, #8331, .T. ) ;
#8241 = AXIS2_PLACEMENT_3D ( 'NONE', #4599, #177, #9229 ) ;
#8242 = CARTESIAN_POINT ( 'NONE',  ( -23.40006363390418187, -133.3880685335015812, 49.99999999999997158 ) ) ;
#8243 = CONICAL_SURFACE ( 'NONE', #7231, 4.025000000000000355, 0.7853981633977258348 ) ;
#8244 = VERTEX_POINT ( 'NONE', #5659 ) ;
#8245 = ADVANCED_FACE ( 'NONE', ( #5759 ), #1754, .F. ) ;
#8246 = DIRECTION ( 'NONE',  ( -1.000000000000000000, -0.000000000000000000, -0.000000000000000000 ) ) ;
#8247 = DIRECTION ( 'NONE',  ( -9.101836848464095537E-17, -0.000000000000000000, -1.000000000000000000 ) ) ;
#8248 = DIRECTION ( 'NONE',  ( 0.000000000000000000, 0.000000000000000000, 1.000000000000000000 ) ) ;
#8249 = CYLINDRICAL_SURFACE ( 'NONE', #7801, 5.000000000000000888 ) ;
#8250 = VECTOR ( 'NONE', #10184, 1000.000000000000000 ) ;
#8251 = CARTESIAN_POINT ( 'NONE',  ( 37.22511195853866894, 17.84145331825996195, 25.00000000000000000 ) ) ;
#8252 = VERTEX_POINT ( 'NONE', #6510 ) ;
#8253 = ORIENTED_EDGE ( 'NONE', *, *, #10086, .T. ) ;
#8254 = AXIS2_PLACEMENT_3D ( 'NONE', #5414, #3085, #6265 ) ;
#8255 = CARTESIAN_POINT ( 'NONE',  ( 3.000000000000000000, 1.467624384280032501, 2.541999999999999371 ) ) ;
#8256 = ORIENTED_EDGE ( 'NONE', *, *, #9951, .F. ) ;
#8257 = DIRECTION ( 'NONE',  ( -0.6691306063588601249, -0.7431448254773928008, 0.000000000000000000 ) ) ;
#8258 = EDGE_CURVE ( 'NONE', #8552, #1166, #4862, .T. ) ;
#8259 = PLANE ( 'NONE',  #5945 ) ;
#8260 = EDGE_CURVE ( 'NONE', #10246, #5184, #5299, .T. ) ;
#8261 = EDGE_CURVE ( 'NONE', #3742, #3983, #9002, .T. ) ;
#8262 = PRESENTATION_STYLE_ASSIGNMENT (( #3436 ) ) ;
#8263 = CARTESIAN_POINT ( 'NONE',  ( -36.36957570605426326, 137.0132282531173473, 0.000000000000000000 ) ) ;
#8264 = DIRECTION ( 'NONE',  ( 1.000000000000000000, 0.000000000000000000, 0.000000000000000000 ) ) ;
#8265 = CIRCLE ( 'NONE', #2005, 2.000000000000001776 ) ;
#8266 = CARTESIAN_POINT ( 'NONE',  ( 39.99999999999997158, -135.1457019118818721, 43.99999999999997158 ) ) ;
#8267 = ORIENTED_EDGE ( 'NONE', *, *, #8050, .T. ) ;
#8268 = AXIS2_PLACEMENT_3D ( 'NONE', #1416, #8934, #6599 ) ;
#8269 = ORIENTED_EDGE ( 'NONE', *, *, #8411, .F. ) ;
#8270 = AXIS2_PLACEMENT_3D ( 'NONE', #2587, #208, #9916 ) ;
#8271 = ORIENTED_EDGE ( 'NONE', *, *, #10145, .F. ) ;
#8272 = CARTESIAN_POINT ( 'NONE',  ( -16.29350689640809691, -140.1746510883711778, 27.01918567566963247 ) ) ;
#8273 = PRESENTATION_STYLE_ASSIGNMENT (( #4919 ) ) ;
#8274 = EDGE_CURVE ( 'NONE', #9740, #2723, #2765, .T. ) ;
#8275 = AXIS2_PLACEMENT_3D ( 'NONE', #4577, #6917, #5215 ) ;
#8276 = CARTESIAN_POINT ( 'NONE',  ( 4.856471286862176662, 145.0444252872335937, 30.00000000000000355 ) ) ;
#8277 = DIRECTION ( 'NONE',  ( 0.000000000000000000, 0.000000000000000000, 1.000000000000000000 ) ) ;
#8278 = DIRECTION ( 'NONE',  ( -1.000000000000000000, -0.000000000000000000, -0.000000000000000000 ) ) ;
#8279 = ORIENTED_EDGE ( 'NONE', *, *, #8402, .T. ) ;
#8280 =( NAMED_UNIT ( * ) SI_UNIT ( $, .STERADIAN. ) SOLID_ANGLE_UNIT ( ) );
#8281 = ORIENTED_EDGE ( 'NONE', *, *, #4463, .F. ) ;
#8282 = CARTESIAN_POINT ( 'NONE',  ( 37.22759939293836595, -115.1457019118818863, -25.15769640663939910 ) ) ;
#8283 = CARTESIAN_POINT ( 'NONE',  ( -23.15769640663937423, -115.1457019118818863, -48.00000000000002132 ) ) ;
#8284 = CARTESIAN_POINT ( 'NONE',  ( 25.15769640663940265, -133.1457019118818721, -48.00000000000002132 ) ) ;
#8285 = CARTESIAN_POINT ( 'NONE',  ( 23.15769640663936713, -117.1457019118819005, 47.99999999999997868 ) ) ;
#8286 = AXIS2_PLACEMENT_3D ( 'NONE', #3810, #627, #5493 ) ;
#8287 = FACE_OUTER_BOUND ( 'NONE', #3909, .T. ) ;
#8288 = ORIENTED_EDGE ( 'NONE', *, *, #1876, .F. ) ;
#8289 = DIRECTION ( 'NONE',  ( 1.000000000000000000, 0.000000000000000000, 0.000000000000000000 ) ) ;
#8290 = ADVANCED_FACE ( 'NONE', ( #370 ), #5337, .T. ) ;
#8291 = ORIENTED_EDGE ( 'NONE', *, *, #868, .T. ) ;
#8292 = DIRECTION ( 'NONE',  ( 0.000000000000000000, 0.000000000000000000, 1.000000000000000000 ) ) ;
#8293 = ORIENTED_EDGE ( 'NONE', *, *, #5218, .T. ) ;
#8294 = VERTEX_POINT ( 'NONE', #2793 ) ;
#8295 = CARTESIAN_POINT ( 'NONE',  ( 99.80027788547049283, -145.1457019118818721, 27.92893218813452094 ) ) ;
#8296 = CARTESIAN_POINT ( 'NONE',  ( -23.76520584195948516, -145.1457019118819005, -97.78965767959371647 ) ) ;
#8297 = PLANE ( 'NONE',  #6860 ) ;
#8298 = DIRECTION ( 'NONE',  ( 1.000000000000000000, -0.000000000000000000, -0.000000000000000000 ) ) ;
#8299 = DIRECTION ( 'NONE',  ( 0.000000000000000000, -1.000000000000000000, 0.000000000000000000 ) ) ;
#8300 = EDGE_CURVE ( 'NONE', #172, #8048, #5136, .T. ) ;
#8301 = ORIENTED_EDGE ( 'NONE', *, *, #8711, .F. ) ;
#8302 = CARTESIAN_POINT ( 'NONE',  ( -11.29350689640808802, 105.5289575273812233, -7.750000000000000888 ) ) ;
#8303 = B_SPLINE_CURVE_WITH_KNOTS ( 'NONE', 3,
 ( #7872, #4691, #10416, #9411 ),
 .UNSPECIFIED., .F., .F.,
 ( 4, 4 ),
 ( 1.430489624538199204E-17, 0.0007942240325546766778 ),
 .UNSPECIFIED. ) ;
#8304 = VECTOR ( 'NONE', #9046, 1000.000000000000000 ) ;
#8305 = ORIENTED_EDGE ( 'NONE', *, *, #10263, .F. ) ;
#8306 = CARTESIAN_POINT ( 'NONE',  ( -2.293506896408097795, 80.56966535057935630, -24.00000000000000711 ) ) ;
#8307 = DIRECTION ( 'NONE',  ( -9.101836848464095537E-17, 0.000000000000000000, -1.000000000000000000 ) ) ;
#8308 = DIRECTION ( 'NONE',  ( 0.000000000000000000, 0.000000000000000000, 1.000000000000000000 ) ) ;
#8309 = LINE ( 'NONE', #4284, #5979 ) ;
#8310 = FACE_OUTER_BOUND ( 'NONE', #6598, .T. ) ;
#8311 = CARTESIAN_POINT ( 'NONE',  ( -16.29350689640809691, 88.12362273389504708, 4.729641367753004033 ) ) ;
#8312 = EDGE_LOOP ( 'NONE', ( #6229, #6297, #1579, #2865 ) ) ;
#8313 = VECTOR ( 'NONE', #2980, 1000.000000000000000 ) ;
#8314 = EDGE_CURVE ( 'NONE', #5783, #3403, #7677, .T. ) ;
#8315 = EDGE_CURVE ( 'NONE', #7894, #8878, #7729, .T. ) ;
#8316 = ORIENTED_EDGE ( 'NONE', *, *, #905, .T. ) ;
#8317 = EDGE_CURVE ( 'NONE', #8095, #1304, #8521, .T. ) ;
#8318 = EDGE_LOOP ( 'NONE', ( #622, #7314, #10175, #792, #3450 ) ) ;
#8319 = CARTESIAN_POINT ( 'NONE',  ( -3.173844575093148990, 105.5289575273812233, 7.750000000000000000 ) ) ;
#8320 = CARTESIAN_POINT ( 'NONE',  ( -16.29350689640809691, -8.660287962196477451, 0.000000000000000000 ) ) ;
#8321 = AXIS2_PLACEMENT_3D ( 'NONE', #1793, #9810, #1686 ) ;
#8322 = CIRCLE ( 'NONE', #5779, 59.51479730733485951 ) ;
#8323 = CARTESIAN_POINT ( 'NONE',  ( 17.97972049165455388, 42.08684478514406635, -30.00000000000000355 ) ) ;
#8324 = DIRECTION ( 'NONE',  ( 0.000000000000000000, 0.000000000000000000, 1.000000000000000000 ) ) ;
#8325 = VERTEX_POINT ( 'NONE', #9158 ) ;
#8326 = DIRECTION ( 'NONE',  ( 0.6691306063588561281, 0.7431448254773961315, 0.000000000000000000 ) ) ;
#8327 = ORIENTED_EDGE ( 'NONE', *, *, #6900, .F. ) ;
#8328 = PRESENTATION_STYLE_ASSIGNMENT (( #5039 ) ) ;
#8329 = PRODUCT_DEFINITION ( 'UNKNOWN', '', #8018, #2612 ) ;
#8330 = AXIS2_PLACEMENT_3D ( 'NONE', #6746, #4936, #8337 ) ;
#8331 = EDGE_CURVE ( 'NONE', #6663, #4985, #2107, .T. ) ;
#8332 = TOROIDAL_SURFACE ( 'NONE', #4768, 4.000000000000000000, 2.000000000000000000 ) ;
#8333 = EDGE_LOOP ( 'NONE', ( #7119, #3048, #243, #2085 ) ) ;
#8334 = DIRECTION ( 'NONE',  ( 0.000000000000000000, 0.000000000000000000, 1.000000000000000000 ) ) ;
#8335 = LINE ( 'NONE', #9131, #28 ) ;
#8336 = DIRECTION ( 'NONE',  ( 0.000000000000000000, -1.000000000000000000, 0.000000000000000000 ) ) ;
#8337 = DIRECTION ( 'NONE',  ( -0.7525569905852205199, -0.6585271261848794078, 0.000000000000000000 ) ) ;
#8338 = AXIS2_PLACEMENT_3D ( 'NONE', #8602, #393, #6103 ) ;
#8339 = DIRECTION ( 'NONE',  ( 0.000000000000000000, 0.000000000000000000, 1.000000000000000000 ) ) ;
#8340 = CARTESIAN_POINT ( 'NONE',  ( -47.94539818030330025, 137.0132282531173473, -3.999999999999991562 ) ) ;
#8341 = VERTEX_POINT ( 'NONE', #8573 ) ;
#8342 = CARTESIAN_POINT ( 'NONE',  ( -24.31850689640809549, 140.5696653505793563, 10.90000000000000036 ) ) ;
#8343 = ORIENTED_EDGE ( 'NONE', *, *, #3146, .T. ) ;
#8344 = AXIS2_PLACEMENT_3D ( 'NONE', #7954, #8746, #10295 ) ;
#8345 = DIRECTION ( 'NONE',  ( 0.000000000000000000, -0.000000000000000000, -1.000000000000000000 ) ) ;
#8346 = EDGE_LOOP ( 'NONE', ( #768, #4298, #7696, #562 ) ) ;
#8347 = EDGE_CURVE ( 'NONE', #10117, #5268, #6486, .T. ) ;
#8348 = CARTESIAN_POINT ( 'NONE',  ( -25.15769640663940621, -117.1457019118819005, 25.15769640663938134 ) ) ;
#8349 = CARTESIAN_POINT ( 'NONE',  ( 37.31363630694986711, -134.7663435696292709, 25.95623500213750035 ) ) ;
#8350 = DIRECTION ( 'NONE',  ( -1.000000000000000000, -0.000000000000000000, -0.000000000000000000 ) ) ;
#8351 = AXIS2_PLACEMENT_3D ( 'NONE', #8263, #3338, #9758 ) ;
#8352 = CARTESIAN_POINT ( 'NONE',  ( -16.29350689640809691, -140.1746510883711778, -30.31717237747080773 ) ) ;
#8353 = ORIENTED_EDGE ( 'NONE', *, *, #4930, .T. ) ;
#8354 = CYLINDRICAL_SURFACE ( 'NONE', #1560, 3.999999999999993339 ) ;
#8355 = DIRECTION ( 'NONE',  ( 1.000000000000000000, 0.000000000000000000, 0.000000000000000000 ) ) ;
#8356 = ORIENTED_EDGE ( 'NONE', *, *, #4194, .F. ) ;
#8357 = CYLINDRICAL_SURFACE ( 'NONE', #2997, 3.999999999999998668 ) ;
#8358 = AXIS2_PLACEMENT_3D ( 'NONE', #628, #726, #3059 ) ;
#8359 = ORIENTED_EDGE ( 'NONE', *, *, #3787, .F. ) ;
#8360 = DIRECTION ( 'NONE',  ( -0.000000000000000000, -0.000000000000000000, 1.000000000000000000 ) ) ;
#8361 = FACE_OUTER_BOUND ( 'NONE', #2541, .T. ) ;
#8362 =( GEOMETRIC_REPRESENTATION_CONTEXT ( 3 ) GLOBAL_UNCERTAINTY_ASSIGNED_CONTEXT ( ( #2506 ) ) GLOBAL_UNIT_ASSIGNED_CONTEXT ( ( #6253, #9494, #9315 ) ) REPRESENTATION_CONTEXT ( 'NONE', 'WORKASPACE' ) );
#8363 = DIRECTION ( 'NONE',  ( 0.000000000000000000, 1.000000000000000000, 0.000000000000000000 ) ) ;
#8364 = DIRECTION ( 'NONE',  ( 0.000000000000000000, 0.000000000000000000, 1.000000000000000000 ) ) ;
#8365 = EDGE_CURVE ( 'NONE', #5357, #6846, #9889, .T. ) ;
#8366 = CARTESIAN_POINT ( 'NONE',  ( -47.94539818030327893, 70.52895752738115220, 0.000000000000000000 ) ) ;
#8367 = LINE ( 'NONE', #950, #6680 ) ;
#8368 = AXIS2_PLACEMENT_3D ( 'NONE', #8392, #9446, #6951 ) ;
#8369 = VERTEX_POINT ( 'NONE', #9216 ) ;
#8370 = ORIENTED_EDGE ( 'NONE', *, *, #10155, .T. ) ;
#8371 = CARTESIAN_POINT ( 'NONE',  ( -20.29350689640809691, 140.5696653505793563, 20.00000000000002132 ) ) ;
#8372 = PLANE ( 'NONE',  #5040 ) ;
#8373 = CARTESIAN_POINT ( 'NONE',  ( -117.0000000000000000, 4.898587196589412829E-16, -4.000000000000000000 ) ) ;
#8374 = AXIS2_PLACEMENT_3D ( 'NONE', #6408, #9555, #1639 ) ;
#8375 = CARTESIAN_POINT ( 'NONE',  ( -3.173844575093148990, 130.5696653505793847, -10.90000000000000036 ) ) ;
#8376 = ADVANCED_FACE ( 'NONE', ( #6134 ), #3706, .T. ) ;
#8377 = FACE_OUTER_BOUND ( 'NONE', #8483, .T. ) ;
#8378 = EDGE_CURVE ( 'NONE', #4419, #415, #8860, .T. ) ;
#8379 = CIRCLE ( 'NONE', #5829, 5.000000000000004441 ) ;
#8380 = VERTEX_POINT ( 'NONE', #3599 ) ;
#8381 = CARTESIAN_POINT ( 'NONE',  ( -1.071796769724492338, 0.000000000000000000, 0.000000000000000000 ) ) ;
#8382 = EDGE_LOOP ( 'NONE', ( #9066, #1167, #10113, #5038 ) ) ;
#8383 = DIRECTION ( 'NONE',  ( 0.000000000000000000, -1.000000000000000000, 0.000000000000000000 ) ) ;
#8384 = ORIENTED_EDGE ( 'NONE', *, *, #9190, .T. ) ;
#8385 = CARTESIAN_POINT ( 'NONE',  ( 6.000000000000005329, 0.000000000000000000, 0.000000000000000000 ) ) ;
#8386 = DIRECTION ( 'NONE',  ( -1.000000000000000000, 0.000000000000000000, 9.101836848464095537E-17 ) ) ;
#8387 = DIRECTION ( 'NONE',  ( 0.000000000000000000, 0.000000000000000000, 1.000000000000000000 ) ) ;
#8388 = DIRECTION ( 'NONE',  ( -1.000000000000000000, -0.000000000000000000, -0.000000000000000000 ) ) ;
#8389 = EDGE_CURVE ( 'NONE', #1931, #9083, #6328, .T. ) ;
#8390 = EDGE_CURVE ( 'NONE', #6365, #1352, #734, .T. ) ;
#8391 = ADVANCED_FACE ( 'NONE', ( #421 ), #10396, .F. ) ;
#8392 = CARTESIAN_POINT ( 'NONE',  ( -16.29350689640809691, -8.660287962196477451, 0.000000000000000000 ) ) ;
#8393 = DIRECTION ( 'NONE',  ( 0.000000000000000000, -0.000000000000000000, -1.000000000000000000 ) ) ;
#8394 = CIRCLE ( 'NONE', #9408, 2.445500000000000007 ) ;
#8395 = ORIENTED_EDGE ( 'NONE', *, *, #9165, .T. ) ;
#8396 = DIRECTION ( 'NONE',  ( -0.000000000000000000, 1.000000000000000000, -0.000000000000000000 ) ) ;
#8397 = ORIENTED_EDGE ( 'NONE', *, *, #884, .T. ) ;
#8398 = TOROIDAL_SURFACE ( 'NONE', #2305, 24.24539146688411506, 5.000000000000000000 ) ;
#8399 = DIRECTION ( 'NONE',  ( 0.000000000000000000, 0.000000000000000000, 1.000000000000000000 ) ) ;
#8400 = ORIENTED_EDGE ( 'NONE', *, *, #3566, .F. ) ;
#8401 = AXIS2_PLACEMENT_3D ( 'NONE', #7861, #5418, #9570 ) ;
#8402 = EDGE_CURVE ( 'NONE', #84, #2663, #10051, .T. ) ;
#8403 = CARTESIAN_POINT ( 'NONE',  ( -40.00000000000001421, -135.1457019118818721, -50.00000000000002132 ) ) ;
#8404 = DIRECTION ( 'NONE',  ( 1.000000000000000000, -0.000000000000000000, -0.000000000000000000 ) ) ;
#8405 = CARTESIAN_POINT ( 'NONE',  ( 14.70649310359190309, 80.56966535057935630, 24.00000000000000711 ) ) ;
#8406 = AXIS2_PLACEMENT_3D ( 'NONE', #8579, #6944, #7052 ) ;
#8407 = ORIENTED_EDGE ( 'NONE', *, *, #6325, .F. ) ;
#8408 = CARTESIAN_POINT ( 'NONE',  ( -56.36957570605427037, 137.0132282531173473, 4.025000000000000355 ) ) ;
#8409 = VECTOR ( 'NONE', #7533, 1000.000000000000000 ) ;
#8410 = SHAPE_REPRESENTATION_RELATIONSHIP ( 'NONE' , 'NONE' ,  #5747, #10381 ) ;
#8411 = EDGE_CURVE ( 'NONE', #2186, #9448, #8184, .T. ) ;
#8412 = ORIENTED_EDGE ( 'NONE', *, *, #4916, .F. ) ;
#8413 = CARTESIAN_POINT ( 'NONE',  ( -16.29350689640809691, -140.1746510883711778, 0.000000000000000000 ) ) ;
#8414 = ORIENTED_EDGE ( 'NONE', *, *, #10135, .F. ) ;
#8415 = DIRECTION ( 'NONE',  ( -0.9973063064792988541, -0.07334937666141910784, 0.000000000000000000 ) ) ;
#8416 = FACE_OUTER_BOUND ( 'NONE', #2998, .T. ) ;
#8417 =( LENGTH_UNIT ( ) NAMED_UNIT ( * ) SI_UNIT ( .MILLI., .METRE. ) );
#8418 = CARTESIAN_POINT ( 'NONE',  ( -16.29350689640809691, -140.1746510883711778, -27.01918567566963247 ) ) ;
#8419 = CARTESIAN_POINT ( 'NONE',  ( -136.5544011653988719, 255.8380805272360590, 1.057583169244835033E-15 ) ) ;
#8420 = CARTESIAN_POINT ( 'NONE',  ( -38.96131932220313132, -0.2735269159956721374, 3.990636919869543942 ) ) ;
#8421 = CIRCLE ( 'NONE', #7077, 4.982234098198590644 ) ;
#8422 = APPLICATION_CONTEXT ( 'automotive_design' ) ;
#8423 = ORIENTED_EDGE ( 'NONE', *, *, #1336, .F. ) ;
#8424 = ADVANCED_FACE ( 'NONE', ( #5130 ), #8523, .F. ) ;
#8425 = ORIENTED_EDGE ( 'NONE', *, *, #8846, .T. ) ;
#8426 = CARTESIAN_POINT ( 'NONE',  ( -40.00000000000001421, -135.1457019118818721, -36.00000000000002842 ) ) ;
#8427 = DIRECTION ( 'NONE',  ( -1.000000000000000000, -0.000000000000000000, -0.000000000000000000 ) ) ;
#8428 = AXIS2_PLACEMENT_3D ( 'NONE', #7014, #5940, #1125 ) ;
#8429 = DIRECTION ( 'NONE',  ( -0.6691306063588565722, -0.7431448254773957984, 0.000000000000000000 ) ) ;
#8430 = DIRECTION ( 'NONE',  ( 0.000000000000000000, 0.000000000000000000, -1.000000000000000000 ) ) ;
#8431 = EDGE_LOOP ( 'NONE', ( #2151, #4288 ) ) ;
#8432 = DIRECTION ( 'NONE',  ( -1.000000000000000000, 0.000000000000000000, 0.000000000000000000 ) ) ;
#8433 = EDGE_LOOP ( 'NONE', ( #4043, #5801, #10057, #8473 ) ) ;
#8434 = DIRECTION ( 'NONE',  ( -1.000000000000000000, -0.000000000000000000, -0.000000000000000000 ) ) ;
#8435 = CIRCLE ( 'NONE', #4201, 7.000000000000016875 ) ;
#8436 = ADVANCED_FACE ( 'NONE', ( #2052 ), #5283, .F. ) ;
#8437 = ORIENTED_EDGE ( 'NONE', *, *, #5270, .T. ) ;
#8438 = DIRECTION ( 'NONE',  ( 0.000000000000000000, 0.000000000000000000, -1.000000000000000000 ) ) ;
#8439 = CARTESIAN_POINT ( 'NONE',  ( -16.29350689640809691, -8.660287962196477451, 0.000000000000000000 ) ) ;
#8440 = CARTESIAN_POINT ( 'NONE',  ( -23.15769640663937423, -117.1457019118819005, -48.00000000000002132 ) ) ;
#8441 = CARTESIAN_POINT ( 'NONE',  ( -16.29350689640809691, -186.9457019118818835, 0.000000000000000000 ) ) ;
#8442 = CARTESIAN_POINT ( 'NONE',  ( -55.94539818030328604, 129.0132282531173757, -3.999999999999990230 ) ) ;
#8443 = EDGE_LOOP ( 'NONE', ( #8683, #8496, #10377, #62 ) ) ;
#8444 = VECTOR ( 'NONE', #9793, 1000.000000000000000 ) ;
#8445 = PLANE ( 'NONE',  #2229 ) ;
#8446 = EDGE_CURVE ( 'NONE', #2463, #8659, #3622, .T. ) ;
#8448 = EDGE_CURVE ( 'NONE', #9513, #6231, #7832, .T. ) ;
#8447 = VERTEX_POINT ( 'NONE', #5390 ) ;
#8449 = EDGE_CURVE ( 'NONE', #6648, #6524, #7683, .T. ) ;
#8450 = DIRECTION ( 'NONE',  ( 0.000000000000000000, 0.000000000000000000, -1.000000000000000000 ) ) ;
#8451 = ORIENTED_EDGE ( 'NONE', *, *, #6630, .F. ) ;
#8452 = VECTOR ( 'NONE', #1894, 1000.000000000000000 ) ;
#8453 = FACE_OUTER_BOUND ( 'NONE', #3997, .T. ) ;
#8454 = CARTESIAN_POINT ( 'NONE',  ( 37.36104957496461765, -134.9117008620985985, 26.18446763346474171 ) ) ;
#8455 = CARTESIAN_POINT ( 'NONE',  ( -45.00000000000000000, 0.000000000000000000, 0.000000000000000000 ) ) ;
#8456 = CYLINDRICAL_SURFACE ( 'NONE', #5438, 4.000000000000000000 ) ;
#8457 = ORIENTED_EDGE ( 'NONE', *, *, #9487, .T. ) ;
#8458 = LINE ( 'NONE', #462, #2249 ) ;
#8459 = ORIENTED_EDGE ( 'NONE', *, *, #1774, .F. ) ;
#8460 = DIRECTION ( 'NONE',  ( 0.000000000000000000, 0.000000000000000000, 1.000000000000000000 ) ) ;
#8461 = ORIENTED_EDGE ( 'NONE', *, *, #8903, .T. ) ;
#8462 = ADVANCED_FACE ( 'NONE', ( #5551 ), #5595, .T. ) ;
#8463 = LINE ( 'NONE', #4588, #8239 ) ;
#8464 = EDGE_CURVE ( 'NONE', #4542, #9316, #2084, .T. ) ;
#8465 = VERTEX_POINT ( 'NONE', #7044 ) ;
#8466 = CARTESIAN_POINT ( 'NONE',  ( 94.81374635307400922, -145.5124487951889876, -25.00000000000000355 ) ) ;
#8467 = FACE_OUTER_BOUND ( 'NONE', #7681, .T. ) ;
#8468 = DIRECTION ( 'NONE',  ( 0.000000000000000000, -1.000000000000000000, 0.000000000000000000 ) ) ;
#8469 = CARTESIAN_POINT ( 'NONE',  ( -23.15769640663940976, -117.1457019118819005, 47.99999999999997868 ) ) ;
#8470 = CARTESIAN_POINT ( 'NONE',  ( -25.15769640663940976, -117.1457019118819005, 47.99999999999997868 ) ) ;
#8471 = CARTESIAN_POINT ( 'NONE',  ( -7.293506896408097795, 120.5696653505793705, -20.00000000000000711 ) ) ;
#8472 = EDGE_LOOP ( 'NONE', ( #10160, #8804 ) ) ;
#8473 = ORIENTED_EDGE ( 'NONE', *, *, #1959, .T. ) ;
#8474 = FACE_OUTER_BOUND ( 'NONE', #1852, .T. ) ;
#8475 = ORIENTED_EDGE ( 'NONE', *, *, #772, .F. ) ;
#8476 = CARTESIAN_POINT ( 'NONE',  ( -30.29350689640809335, 120.5696653505793705, -20.00000000000000711 ) ) ;
#8477 = LINE ( 'NONE', #6781, #2064 ) ;
#8478 = FACE_OUTER_BOUND ( 'NONE', #1916, .T. ) ;
#8479 = EDGE_CURVE ( 'NONE', #4826, #8668, #4134, .T. ) ;
#8480 = FACE_OUTER_BOUND ( 'NONE', #2900, .T. ) ;
#8481 = VECTOR ( 'NONE', #6672, 1000.000000000000000 ) ;
#8482 = ORIENTED_EDGE ( 'NONE', *, *, #10070, .T. ) ;
#8483 = EDGE_LOOP ( 'NONE', ( #9764, #5091, #9805, #7024 ) ) ;
#8484 = DIRECTION ( 'NONE',  ( 8.659560562356134638E-17, 0.7071067811864494290, -0.7071067811866454944 ) ) ;
#8485 = CIRCLE ( 'NONE', #4761, 7.999999999999996447 ) ;
#8486 = ORIENTED_EDGE ( 'NONE', *, *, #10398, .F. ) ;
#8487 = VECTOR ( 'NONE', #8490, 1000.000000000000000 ) ;
#8488 = ORIENTED_EDGE ( 'NONE', *, *, #8967, .T. ) ;
#8489 = PLANE ( 'NONE',  #8428 ) ;
#8490 = DIRECTION ( 'NONE',  ( -1.396588258780021135E-16, -0.000000000000000000, 1.000000000000000000 ) ) ;
#8491 = CARTESIAN_POINT ( 'NONE',  ( -48.00000000000002132, -133.1457019118818721, -25.15769640663945950 ) ) ;
#8492 = CARTESIAN_POINT ( 'NONE',  ( 1.940506014114293224E-14, -115.1457019118818863, -23.15769640663941331 ) ) ;
#8493 = ADVANCED_FACE ( 'NONE', ( #8786 ), #8626, .T. ) ;
#8494 = FACE_OUTER_BOUND ( 'NONE', #2372, .T. ) ;
#8495 = VECTOR ( 'NONE', #9372, 1000.000000000000000 ) ;
#8496 = ORIENTED_EDGE ( 'NONE', *, *, #1453, .T. ) ;
#8497 = VECTOR ( 'NONE', #8427, 1000.000000000000000 ) ;
#8498 = CARTESIAN_POINT ( 'NONE',  ( -144.3499457102809913, 273.6050080517225638, 2.035728505737848743E-15 ) ) ;
#8499 = DIRECTION ( 'NONE',  ( 0.000000000000000000, -1.000000000000000000, -9.100899318238108411E-17 ) ) ;
#8500 = CARTESIAN_POINT ( 'NONE',  ( 99.80027788547049283, -145.1457019118819005, 30.00000000000000355 ) ) ;
#8501 = VECTOR ( 'NONE', #2444, 1000.000000000000000 ) ;
#8502 = VECTOR ( 'NONE', #5587, 1000.000000000000000 ) ;
#8503 = LINE ( 'NONE', #455, #7073 ) ;
#8504 = CARTESIAN_POINT ( 'NONE',  ( 37.26943424014034889, -134.4902506524434500, 25.67119517670793627 ) ) ;
#8505 = EDGE_CURVE ( 'NONE', #836, #9808, #73, .T. ) ;
#8506 = DIRECTION ( 'NONE',  ( -0.7431448254773957984, 0.6691306063588564612, 0.000000000000000000 ) ) ;
#8507 = ADVANCED_FACE ( 'NONE', ( #9429 ), #8866, .T. ) ;
#8508 = EDGE_CURVE ( 'NONE', #3326, #2357, #6290, .T. ) ;
#8509 = CARTESIAN_POINT ( 'NONE',  ( -163.4029438717997209, 273.7745032373030085, 4.898587196589412829E-16 ) ) ;
#8510 = ORIENTED_EDGE ( 'NONE', *, *, #2684, .F. ) ;
#8511 = CARTESIAN_POINT ( 'NONE',  ( -40.00000000000001421, -135.1707019118818778, -44.00000000000002132 ) ) ;
#8512 = CONICAL_SURFACE ( 'NONE', #1576, 4.025000000000000355, 0.7853981633975870569 ) ;
#8513 = ORIENTED_EDGE ( 'NONE', *, *, #9890, .F. ) ;
#8514 = SHAPE_REPRESENTATION_RELATIONSHIP ( 'NONE' , 'NONE' ,  #6905, #3680 ) ;
#8515 = EDGE_LOOP ( 'NONE', ( #176, #3657, #9149, #6236, #3029, #3819, #7958, #3373, #8116, #4388 ) ) ;
#8516 = CARTESIAN_POINT ( 'NONE',  ( 25.15769640663936357, -133.1457019118818721, 27.15769640663938489 ) ) ;
#8517 = ORIENTED_EDGE ( 'NONE', *, *, #8653, .F. ) ;
#8518 = EDGE_LOOP ( 'NONE', ( #4764, #2611, #3647, #8222 ) ) ;
#8519 = DIRECTION ( 'NONE',  ( -0.000000000000000000, 0.000000000000000000, -1.000000000000000000 ) ) ;
#8520 = DIRECTION ( 'NONE',  ( 0.000000000000000000, 0.000000000000000000, 1.000000000000000000 ) ) ;
#8521 = CIRCLE ( 'NONE', #574, 2.000000000000001776 ) ;
#8522 = DIRECTION ( 'NONE',  ( 0.000000000000000000, -1.000000000000000000, 0.000000000000000000 ) ) ;
#8523 = CYLINDRICAL_SURFACE ( 'NONE', #6659, 3.999999999999989786 ) ;
#8524 = PRODUCT_DEFINITION ( 'UNKNOWN', '', #7182, #5044 ) ;
#8525 = EDGE_CURVE ( 'NONE', #2815, #2514, #9723, .T. ) ;
#8526 = CARTESIAN_POINT ( 'NONE',  ( 5.999999999999998224, 0.000000000000000000, 0.000000000000000000 ) ) ;
#8527 = EDGE_CURVE ( 'NONE', #2342, #6087, #2772, .T. ) ;
#8528 = CARTESIAN_POINT ( 'NONE',  ( -39.00000000000000000, 3.117691453623999909, -1.799999999999972733 ) ) ;
#8529 = ORIENTED_EDGE ( 'NONE', *, *, #5599, .F. ) ;
#8530 = ORIENTED_EDGE ( 'NONE', *, *, #4516, .T. ) ;
#8531 = AXIS2_PLACEMENT_3D ( 'NONE', #576, #3866, #3916 ) ;
#8532 = DIRECTION ( 'NONE',  ( -7.493424318096922963E-17, 0.9063077870366528233, -0.4226182617406935016 ) ) ;
#8533 = ORIENTED_EDGE ( 'NONE', *, *, #7928, .F. ) ;
#8534 = LINE ( 'NONE', #2755, #4378 ) ;
#8535 = DIRECTION ( 'NONE',  ( 8.659560562355533132E-17, -0.7071067811864985009, 0.7071067811865965336 ) ) ;
#8536 = CARTESIAN_POINT ( 'NONE',  ( -50.00000000000002132, -135.1457019118818721, -6.938893903907231533E-15 ) ) ;
#8537 = DIRECTION ( 'NONE',  ( -7.016001027857731783E-17, 0.8191520442889911324, -0.5735764363510471586 ) ) ;
#8538 = ADVANCED_FACE ( 'NONE', ( #2959 ), #2271, .F. ) ;
#8539 = ORIENTED_EDGE ( 'NONE', *, *, #4405, .T. ) ;
#8540 = ORIENTED_EDGE ( 'NONE', *, *, #5919, .F. ) ;
#8541 = EDGE_CURVE ( 'NONE', #7514, #5742, #2940, .T. ) ;
#8542 = VECTOR ( 'NONE', #9787, 1000.000000000000000 ) ;
#8543 = ORIENTED_EDGE ( 'NONE', *, *, #6529, .F. ) ;
#8544 = ORIENTED_EDGE ( 'NONE', *, *, #6276, .T. ) ;
#8545 = ORIENTED_EDGE ( 'NONE', *, *, #2682, .T. ) ;
#8546 = DIRECTION ( 'NONE',  ( 0.000000000000000000, -1.000000000000000000, -9.100899318238108411E-17 ) ) ;
#8547 = LINE ( 'NONE', #8600, #8313 ) ;
#8548 = AXIS2_PLACEMENT_3D ( 'NONE', #6723, #9974, #2481 ) ;
#8549 = DIRECTION ( 'NONE',  ( -0.000000000000000000, -0.000000000000000000, 1.000000000000000000 ) ) ;
#8550 = DIRECTION ( 'NONE',  ( 0.000000000000000000, 0.000000000000000000, 1.000000000000000000 ) ) ;
#8551 = DIRECTION ( 'NONE',  ( 1.000000000000000000, 0.000000000000000000, 0.000000000000000000 ) ) ;
#8552 = VERTEX_POINT ( 'NONE', #8831 ) ;
#8553 = CARTESIAN_POINT ( 'NONE',  ( -40.00000000000002842, -135.1457019118818721, 39.99999999999997868 ) ) ;
#8554 = CARTESIAN_POINT ( 'NONE',  ( -7.293506896408097795, 120.5696653505793705, -28.00000000000000355 ) ) ;
#8555 = ORIENTED_EDGE ( 'NONE', *, *, #1124, .F. ) ;
#8556 = VECTOR ( 'NONE', #6170, 1000.000000000000000 ) ;
#8557 = LINE ( 'NONE', #4636, #10110 ) ;
#8558 = CARTESIAN_POINT ( 'NONE',  ( 27.15769640663938489, -133.1457019118818721, -27.15769640663940976 ) ) ;
#8559 = CARTESIAN_POINT ( 'NONE',  ( 14.70649310359190309, 80.56966535057935630, -24.00000000000000711 ) ) ;
#8560 = ORIENTED_EDGE ( 'NONE', *, *, #3760, .T. ) ;
#8561 = CARTESIAN_POINT ( 'NONE',  ( 27.15769640663938489, -117.1457019118819005, -25.15769640663940621 ) ) ;
#8562 = ORIENTED_EDGE ( 'NONE', *, *, #7540, .F. ) ;
#8563 = ORIENTED_EDGE ( 'NONE', *, *, #7336, .F. ) ;
#8564 = VECTOR ( 'NONE', #4524, 1000.000000000000000 ) ;
#8565 = DIRECTION ( 'NONE',  ( -0.000000000000000000, -0.000000000000000000, -1.000000000000000000 ) ) ;
#8566 = EDGE_CURVE ( 'NONE', #7848, #4047, #4796, .T. ) ;
#8567 = VERTEX_POINT ( 'NONE', #5494 ) ;
#8568 = ORIENTED_EDGE ( 'NONE', *, *, #4238, .T. ) ;
#8569 = CARTESIAN_POINT ( 'NONE',  ( -16.29350689640809691, 105.5289575273812233, -10.90000000000000036 ) ) ;
#8570 = CARTESIAN_POINT ( 'NONE',  ( -54.56278605312611774, 170.3918540369290895, 0.000000000000000000 ) ) ;
#8571 = AXIS2_PLACEMENT_3D ( 'NONE', #3188, #8009, #2295 ) ;
#8572 = DIRECTION ( 'NONE',  ( -0.000000000000000000, -0.000000000000000000, -1.000000000000000000 ) ) ;
#8573 = CARTESIAN_POINT ( 'NONE',  ( -23.76520584195948516, -145.1457019118819005, 0.6509338422959615178 ) ) ;
#8574 = FACE_OUTER_BOUND ( 'NONE', #8472, .T. ) ;
#8575 = CIRCLE ( 'NONE', #4009, 3.999999999999998668 ) ;
#8576 = LINE ( 'NONE', #6083, #6784 ) ;
#8577 = VERTEX_POINT ( 'NONE', #6185 ) ;
#8578 = VECTOR ( 'NONE', #1536, 1000.000000000000000 ) ;
#8579 = CARTESIAN_POINT ( 'NONE',  ( -56.36957570605426326, 90.52895752738122326, 10.90000000000000036 ) ) ;
#8580 = EDGE_CURVE ( 'NONE', #8605, #9452, #10059, .T. ) ;
#8581 = ADVANCED_FACE ( 'NONE', ( #4166 ), #4064, .F. ) ;
#8582 = EDGE_CURVE ( 'NONE', #3508, #3785, #5646, .T. ) ;
#8583 = VECTOR ( 'NONE', #2576, 1000.000000000000000 ) ;
#8584 = ORIENTED_EDGE ( 'NONE', *, *, #4309, .F. ) ;
#8585 = FACE_OUTER_BOUND ( 'NONE', #8774, .T. ) ;
#8586 = CARTESIAN_POINT ( 'NONE',  ( 0.000000000000000000, 0.000000000000000000, 0.000000000000000000 ) ) ;
#8587 = VERTEX_POINT ( 'NONE', #8884 ) ;
#8588 = CYLINDRICAL_SURFACE ( 'NONE', #9881, 3.297986701801175258 ) ;
#8589 = DIRECTION ( 'NONE',  ( -7.493424318096921731E-17, 0.9063077870366529343, -0.4226182617406935016 ) ) ;
#8590 = AXIS2_PLACEMENT_3D ( 'NONE', #4477, #3949, #5678 ) ;
#8591 = FACE_BOUND ( 'NONE', #781, .T. ) ;
#8592 = ORIENTED_EDGE ( 'NONE', *, *, #8464, .T. ) ;
#8593 = ORIENTED_EDGE ( 'NONE', *, *, #1843, .T. ) ;
#8594 = CIRCLE ( 'NONE', #1652, 0.2500000000000002220 ) ;
#8595 = VECTOR ( 'NONE', #4098, 1000.000000000000000 ) ;
#8596 = ORIENTED_EDGE ( 'NONE', *, *, #225, .T. ) ;
#8597 = EDGE_CURVE ( 'NONE', #7029, #2154, #9351, .T. ) ;
#8598 = EDGE_LOOP ( 'NONE', ( #464, #2881 ) ) ;
#8599 = LINE ( 'NONE', #1181, #7925 ) ;
#8600 = CARTESIAN_POINT ( 'NONE',  ( 4.856471286862173997, 152.5696653505793279, 25.00000000000000000 ) ) ;
#8601 = DIRECTION ( 'NONE',  ( 1.000000000000000000, 0.000000000000000000, 0.000000000000000000 ) ) ;
#8602 = CARTESIAN_POINT ( 'NONE',  ( -16.29350689640809691, 81.26698356513965393, 0.000000000000000000 ) ) ;
#8603 = PLANE ( 'NONE',  #8234 ) ;
#8604 = CIRCLE ( 'NONE', #9110, 2.000000000000001776 ) ;
#8605 = VERTEX_POINT ( 'NONE', #932 ) ;
#8606 = DIRECTION ( 'NONE',  ( -0.7431448254773957984, 0.6691306063588564612, 0.000000000000000000 ) ) ;
#8607 = VECTOR ( 'NONE', #9847, 1000.000000000000000 ) ;
#8608 = CARTESIAN_POINT ( 'NONE',  ( 2.275687196221499263E-14, -133.1457019118818721, -27.15769640663943107 ) ) ;
#8609 = ORIENTED_EDGE ( 'NONE', *, *, #4285, .F. ) ;
#8610 = CARTESIAN_POINT ( 'NONE',  ( -38.99999999999999289, -5.592496027482437178E-16, 3.600000000000004530 ) ) ;
#8611 = AXIS2_PLACEMENT_3D ( 'NONE', #5777, #9721, #911 ) ;
#8612 = LINE ( 'NONE', #7027, #6848 ) ;
#8613 = EDGE_CURVE ( 'NONE', #8605, #8567, #774, .T. ) ;
#8614 = FACE_OUTER_BOUND ( 'NONE', #3961, .T. ) ;
#8615 = ORIENTED_EDGE ( 'NONE', *, *, #1974, .T. ) ;
#8616 = CYLINDRICAL_SURFACE ( 'NONE', #2401, 7.500000000000000000 ) ;
#8617 = PRODUCT_CONTEXT ( 'NONE', #8422, 'mechanical' ) ;
#8618 = VERTEX_POINT ( 'NONE', #1729 ) ;
#8619 = FACE_OUTER_BOUND ( 'NONE', #2973, .T. ) ;
#8620 = ORIENTED_EDGE ( 'NONE', *, *, #240, .T. ) ;
#8621 = ORIENTED_EDGE ( 'NONE', *, *, #7750, .T. ) ;
#8622 = CARTESIAN_POINT ( 'NONE',  ( -16.29350689640809691, 88.12362273389504708, -4.729641367753004033 ) ) ;
#8623 = DIRECTION ( 'NONE',  ( -0.000000000000000000, -1.000000000000000000, -0.000000000000000000 ) ) ;
#8624 = ORIENTED_EDGE ( 'NONE', *, *, #3225, .T. ) ;
#8625 = FILL_AREA_STYLE_COLOUR ( '', #2327 ) ;
#8626 = CYLINDRICAL_SURFACE ( 'NONE', #3118, 5.000000000000000888 ) ;
#8627 = DIRECTION ( 'NONE',  ( 0.000000000000000000, -1.000000000000000000, 0.000000000000000000 ) ) ;
#8628 = DIRECTION ( 'NONE',  ( -0.000000000000000000, -0.000000000000000000, -1.000000000000000000 ) ) ;
#8629 = CARTESIAN_POINT ( 'NONE',  ( -40.99999999999999289, 3.464101615137777923, -1.999999999999970468 ) ) ;
#8630 = EDGE_CURVE ( 'NONE', #6245, #6390, #245, .T. ) ;
#8631 = EDGE_LOOP ( 'NONE', ( #3123, #9146, #2140 ) ) ;
#8632 = DIRECTION ( 'NONE',  ( 0.000000000000000000, -1.000000000000000000, 0.000000000000000000 ) ) ;
#8633 = VERTEX_POINT ( 'NONE', #8193 ) ;
#8634 = LINE ( 'NONE', #7001, #1161 ) ;
#8635 = CARTESIAN_POINT ( 'NONE',  ( -16.29350689640810756, 140.5696653505793563, 20.00000000000002132 ) ) ;
#8636 = DIRECTION ( 'NONE',  ( 0.000000000000000000, 0.000000000000000000, -1.000000000000000000 ) ) ;
#8637 = FACE_OUTER_BOUND ( 'NONE', #9426, .T. ) ;
#8638 = FACE_OUTER_BOUND ( 'NONE', #2976, .T. ) ;
#8639 = VERTEX_POINT ( 'NONE', #4016 ) ;
#8640 = EDGE_CURVE ( 'NONE', #477, #8380, #2090, .T. ) ;
#8641 = EDGE_CURVE ( 'NONE', #9924, #5289, #912, .T. ) ;
#8642 = EDGE_CURVE ( 'NONE', #2784, #1166, #7401, .T. ) ;
#8643 = EDGE_LOOP ( 'NONE', ( #10412, #2011, #6726, #2100 ) ) ;
#8644 = PRODUCT_DEFINITION_SHAPE ( 'NONE', 'NONE',  #8197 ) ;
#8645 = ORIENTED_EDGE ( 'NONE', *, *, #5271, .T. ) ;
#8646 = ORIENTED_EDGE ( 'NONE', *, *, #3081, .T. ) ;
#8647 = DIRECTION ( 'NONE',  ( -0.000000000000000000, 1.000000000000000000, -0.000000000000000000 ) ) ;
#8648 = CARTESIAN_POINT ( 'NONE',  ( 99.80027788547049283, -145.1457019118819005, -25.00000000000000355 ) ) ;
#8649 = AXIS2_PLACEMENT_3D ( 'NONE', #5183, #523, #1162 ) ;
#8650 = FACE_OUTER_BOUND ( 'NONE', #7862, .T. ) ;
#8651 = LINE ( 'NONE', #3782, #6472 ) ;
#8652 = DIRECTION ( 'NONE',  ( 0.000000000000000000, 0.000000000000000000, -1.000000000000000000 ) ) ;
#8653 = EDGE_CURVE ( 'NONE', #9336, #9263, #582, .T. ) ;
#8654 = EDGE_LOOP ( 'NONE', ( #5125, #280, #7556, #76 ) ) ;
#8655 = DIRECTION ( 'NONE',  ( -0.000000000000000000, -0.000000000000000000, 1.000000000000000000 ) ) ;
#8656 = AXIS2_PLACEMENT_3D ( 'NONE', #4737, #10472, #9413 ) ;
#8657 = PRESENTATION_LAYER_ASSIGNMENT (  '', '', ( #9163 ) ) ;
#8658 = VERTEX_POINT ( 'NONE', #9852 ) ;
#8659 = VERTEX_POINT ( 'NONE', #7247 ) ;
#8660 = VECTOR ( 'NONE', #9657, 1000.000000000000000 ) ;
#8661 = CARTESIAN_POINT ( 'NONE',  ( 37.59878849545336266, 37.08684478514405214, 12.50000000000000000 ) ) ;
#8662 = AXIS2_PLACEMENT_3D ( 'NONE', #4676, #6416, #4820 ) ;
#8663 = CARTESIAN_POINT ( 'NONE',  ( -20.29350689640809691, 140.5696653505793563, 10.98204862120179826 ) ) ;
#8664 = CARTESIAN_POINT ( 'NONE',  ( 23.15769640663940265, -117.1457019118819005, -50.00000000000002132 ) ) ;
#8665 = ORIENTED_EDGE ( 'NONE', *, *, #8640, .F. ) ;
#8666 = CARTESIAN_POINT ( 'NONE',  ( 39.99999999999998579, -135.1457019118818721, -50.00000000000002132 ) ) ;
#8667 = CARTESIAN_POINT ( 'NONE',  ( -36.29350689640810401, 120.5696653505793705, 20.00000000000000711 ) ) ;
#8668 = VERTEX_POINT ( 'NONE', #5804 ) ;
#8669 = CIRCLE ( 'NONE', #4434, 2.000000000000001776 ) ;
#8670 = DIRECTION ( 'NONE',  ( 1.000000000000000000, -0.000000000000000000, -0.000000000000000000 ) ) ;
#8671 = ORIENTED_EDGE ( 'NONE', *, *, #4929, .F. ) ;
#8672 = ADVANCED_FACE ( 'NONE', ( #986, #150 ), #3264, .F. ) ;
#8673 = ORIENTED_EDGE ( 'NONE', *, *, #6324, .T. ) ;
#8674 = CARTESIAN_POINT ( 'NONE',  ( -18.34874108452141783, -140.1746510883711778, 29.59847408863694440 ) ) ;
#8675 = LINE ( 'NONE', #8729, #3601 ) ;
#8676 = PLANE ( 'NONE',  #1010 ) ;
#8677 = DIRECTION ( 'NONE',  ( -0.000000000000000000, -0.000000000000000000, 1.000000000000000000 ) ) ;
#8678 = CARTESIAN_POINT ( 'NONE',  ( -43.21545076107636874, 261.9011211458127377, 9.258022131055327982E-15 ) ) ;
#8679 = AXIS2_PLACEMENT_3D ( 'NONE', #4623, #2027, #5254 ) ;
#8680 = DIRECTION ( 'NONE',  ( 1.000000000000000000, 1.748065976125624994E-15, 0.000000000000000000 ) ) ;
#8681 = VECTOR ( 'NONE', #8396, 1000.000000000000000 ) ;
#8682 = DIRECTION ( 'NONE',  ( -6.964995403156261684E-17, -0.08715574274766943463, 0.9961946980917445460 ) ) ;
#8683 = ORIENTED_EDGE ( 'NONE', *, *, #868, .F. ) ;
#8684 = DIRECTION ( 'NONE',  ( -1.000000000000000000, 0.000000000000000000, 0.000000000000000000 ) ) ;
#8685 = VECTOR ( 'NONE', #4921, 1000.000000000000000 ) ;
#8686 = ORIENTED_EDGE ( 'NONE', *, *, #4012, .T. ) ;
#8687 = EDGE_CURVE ( 'NONE', #10117, #6043, #1677, .T. ) ;
#8688 = CARTESIAN_POINT ( 'NONE',  ( -40.00000000000001421, -145.1457019118819005, -50.00000000000002132 ) ) ;
#8689 = FACE_OUTER_BOUND ( 'NONE', #3107, .T. ) ;
#8690 = LINE ( 'NONE', #10391, #399 ) ;
#8691 = CARTESIAN_POINT ( 'NONE',  ( -7.293506896408097795, 4.007378841484243628E-15, 28.00000000000002132 ) ) ;
#8692 = DIRECTION ( 'NONE',  ( -0.6691306063588565722, -0.7431448254773957984, 0.000000000000000000 ) ) ;
#8693 = ORIENTED_EDGE ( 'NONE', *, *, #6662, .F. ) ;
#8694 = VECTOR ( 'NONE', #5022, 1000.000000000000000 ) ;
#8695 = ORIENTED_EDGE ( 'NONE', *, *, #3139, .T. ) ;
#8696 = EDGE_CURVE ( 'NONE', #996, #2723, #3630, .T. ) ;
#8697 = EDGE_LOOP ( 'NONE', ( #10060, #5316, #4923, #9032 ) ) ;
#8698 = ORIENTED_EDGE ( 'NONE', *, *, #4050, .F. ) ;
#8699 = EDGE_CURVE ( 'NONE', #5224, #2732, #7692, .T. ) ;
#8700 = CARTESIAN_POINT ( 'NONE',  ( -23.15769640663937423, -133.1457019118818721, -50.00000000000002132 ) ) ;
#8701 = DIRECTION ( 'NONE',  ( 0.000000000000000000, 0.000000000000000000, -1.000000000000000000 ) ) ;
#8702 = AXIS2_PLACEMENT_3D ( 'NONE', #9482, #9539, #7940 ) ;
#8703 = EDGE_CURVE ( 'NONE', #1800, #9582, #10232, .T. ) ;
#8704 = PLANE ( 'NONE',  #8913 ) ;
#8705 = DIRECTION ( 'NONE',  ( 0.000000000000000000, 0.000000000000000000, -1.000000000000000000 ) ) ;
#8706 = CYLINDRICAL_SURFACE ( 'NONE', #4001, 7.999999999999989342 ) ;
#8707 = ORIENTED_EDGE ( 'NONE', *, *, #6866, .T. ) ;
#8708 = LINE ( 'NONE', #7021, #4615 ) ;
#8709 = CIRCLE ( 'NONE', #7695, 5.025000000000002132 ) ;
#8710 = EDGE_LOOP ( 'NONE', ( #6424, #5408, #2840, #1724, #9952, #8013 ) ) ;
#8711 = EDGE_CURVE ( 'NONE', #4318, #869, #1591, .T. ) ;
#8712 = DIRECTION ( 'NONE',  ( 0.000000000000000000, -0.5000000000000012212, -0.8660254037844380415 ) ) ;
#8713 = ADVANCED_FACE ( 'NONE', ( #828 ), #9044, .T. ) ;
#8714 = ADVANCED_FACE ( 'NONE', ( #5165 ), #2087, .F. ) ;
#8715 = CIRCLE ( 'NONE', #1604, 3.999999999999989786 ) ;
#8716 = PLANE ( 'NONE',  #963 ) ;
#8717 = DIRECTION ( 'NONE',  ( 0.000000000000000000, 0.4999999999999985567, -0.8660254037844394848 ) ) ;
#8718 = DIRECTION ( 'NONE',  ( -1.277197683604454965E-16, 1.000000000000000000, 0.000000000000000000 ) ) ;
#8719 = ORIENTED_EDGE ( 'NONE', *, *, #9261, .T. ) ;
#8720 = AXIS2_PLACEMENT_3D ( 'NONE', #4967, #213, #1638 ) ;
#8721 = FACE_OUTER_BOUND ( 'NONE', #3316, .T. ) ;
#8722 = APPLICATION_PROTOCOL_DEFINITION ( 'draft international standard', 'automotive_design', 1998, #8422 ) ;
#8723 = ORIENTED_EDGE ( 'NONE', *, *, #4311, .T. ) ;
#8724 = DIRECTION ( 'NONE',  ( 0.000000000000000000, 0.000000000000000000, 1.000000000000000000 ) ) ;
#8725 = ORIENTED_EDGE ( 'NONE', *, *, #274, .T. ) ;
#8726 = AXIS2_PLACEMENT_3D ( 'NONE', #775, #10431, #3812 ) ;
#8727 = ADVANCED_FACE ( 'NONE', ( #6708 ), #1035, .F. ) ;
#8728 = DIRECTION ( 'NONE',  ( 0.000000000000000000, 0.000000000000000000, -1.000000000000000000 ) ) ;
#8729 = CARTESIAN_POINT ( 'NONE',  ( 77.30044127146540234, 73.68369600860394542, 30.00000000000000355 ) ) ;
#8730 = DIRECTION ( 'NONE',  ( 1.000000000000000000, -0.000000000000000000, -0.000000000000000000 ) ) ;
#8731 = CARTESIAN_POINT ( 'NONE',  ( 4.856471286862176662, 145.0444252872335937, -25.00000000000003197 ) ) ;
#8732 = CARTESIAN_POINT ( 'NONE',  ( 26.00000000000000355, 2.445500000000000007, 0.000000000000000000 ) ) ;
#8733 = AXIS2_PLACEMENT_3D ( 'NONE', #10428, #2103, #1419 ) ;
#8734 = PLANE ( 'NONE',  #8989 ) ;
#8735 = CARTESIAN_POINT ( 'NONE',  ( -37.01000625782472753, 0.000000000000000000, 0.000000000000000000 ) ) ;
#8736 = EDGE_CURVE ( 'NONE', #9477, #1670, #3580, .T. ) ;
#8737 = AXIS2_PLACEMENT_3D ( 'NONE', #1517, #2256, #8773 ) ;
#8738 = VERTEX_POINT ( 'NONE', #2728 ) ;
#8739 = CARTESIAN_POINT ( 'NONE',  ( -23.76520584195948516, -145.1457019118819005, -0.6509338422960262438 ) ) ;
#8740 = VECTOR ( 'NONE', #1598, 1000.000000000000000 ) ;
#8741 = VERTEX_POINT ( 'NONE', #1989 ) ;
#8742 = CARTESIAN_POINT ( 'NONE',  ( -48.00000000000002132, -117.1457019118819005, -6.661338147750942398E-15 ) ) ;
#8743 = CARTESIAN_POINT ( 'NONE',  ( -3.173844575093148990, 130.5696653505793847, 10.90000000000000036 ) ) ;
#8744 = AXIS2_PLACEMENT_3D ( 'NONE', #6594, #10470, #9031 ) ;
#8745 = ORIENTED_EDGE ( 'NONE', *, *, #1078, .T. ) ;
#8746 = DIRECTION ( 'NONE',  ( -0.000000000000000000, -1.000000000000000000, -0.000000000000000000 ) ) ;
#8747 = CARTESIAN_POINT ( 'NONE',  ( -16.29350689640809691, -8.660287962196477451, 0.000000000000000000 ) ) ;
#8748 = FACE_OUTER_BOUND ( 'NONE', #1467, .T. ) ;
#8749 = EDGE_LOOP ( 'NONE', ( #8214, #2517, #10188, #5014 ) ) ;
#8750 = ADVANCED_FACE ( 'NONE', ( #1193 ), #353, .F. ) ;
#8751 = AXIS2_PLACEMENT_3D ( 'NONE', #4856, #8945, #8891 ) ;
#8752 = ORIENTED_EDGE ( 'NONE', *, *, #2845, .T. ) ;
#8753 = AXIS2_PLACEMENT_3D ( 'NONE', #8970, #1601, #14 ) ;
#8754 = AXIS2_PLACEMENT_3D ( 'NONE', #931, #4165, #7400 ) ;
#8755 = ORIENTED_EDGE ( 'NONE', *, *, #3131, .F. ) ;
#8756 = FACE_OUTER_BOUND ( 'NONE', #4264, .T. ) ;
#8757 = CARTESIAN_POINT ( 'NONE',  ( -30.29350689640809335, 37.08684478514406635, -15.00000000000000355 ) ) ;
#8758 = CLOSED_SHELL ( 'NONE', ( #5205, #3790, #2750, #7277, #7941, #4756, #9167, #8979, #6984, #2385, #5220 ) ) ;
#8759 = DIRECTION ( 'NONE',  ( 0.000000000000000000, 0.000000000000000000, 1.000000000000000000 ) ) ;
#8760 = DIRECTION ( 'NONE',  ( 6.106226635438360972E-16, -1.000000000000000000, 0.000000000000000000 ) ) ;
#8761 = VECTOR ( 'NONE', #9226, 1000.000000000000000 ) ;
#8762 = CARTESIAN_POINT ( 'NONE',  ( 0.000000000000000000, -135.1457019118818721, -50.00000000000002132 ) ) ;
#8763 = ORIENTED_EDGE ( 'NONE', *, *, #3149, .F. ) ;
#8764 = DIRECTION ( 'NONE',  ( 0.000000000000000000, 0.000000000000000000, 1.000000000000000000 ) ) ;
#8765 = EDGE_CURVE ( 'NONE', #2586, #3286, #10222, .T. ) ;
#8766 = AXIS2_PLACEMENT_3D ( 'NONE', #8229, #8923, #6534 ) ;
#8767 = VERTEX_POINT ( 'NONE', #6116 ) ;
#8768 = AXIS2_PLACEMENT_3D ( 'NONE', #1588, #1436, #6358 ) ;
#8769 = CARTESIAN_POINT ( 'NONE',  ( 0.000000000000000000, 2.935248768560057897, -3.252606517456513302E-15 ) ) ;
#8770 = AXIS2_PLACEMENT_3D ( 'NONE', #586, #10236, #2174 ) ;
#8771 = FACE_OUTER_BOUND ( 'NONE', #1910, .T. ) ;
#8772 = CARTESIAN_POINT ( 'NONE',  ( 24.15110854952564168, -134.0910177696405299, -50.00000000000002132 ) ) ;
#8773 = DIRECTION ( 'NONE',  ( 0.000000000000000000, 0.000000000000000000, 1.000000000000000000 ) ) ;
#8774 = EDGE_LOOP ( 'NONE', ( #8922, #8782, #5716, #359, #6013 ) ) ;
#8775 = EDGE_CURVE ( 'NONE', #2946, #3592, #9898, .T. ) ;
#8776 = ADVANCED_FACE ( 'NONE', ( #5957 ), #3970, .F. ) ;
#8777 = ADVANCED_FACE ( 'NONE', ( #5906 ), #308, .T. ) ;
#8778 = APPLICATION_PROTOCOL_DEFINITION ( 'draft international standard', 'automotive_design', 1998, #1525 ) ;
#8779 = ORIENTED_EDGE ( 'NONE', *, *, #1987, .F. ) ;
#8780 = VECTOR ( 'NONE', #942, 1000.000000000000000 ) ;
#8781 = DIRECTION ( 'NONE',  ( -0.000000000000000000, 0.000000000000000000, 1.000000000000000000 ) ) ;
#8782 = ORIENTED_EDGE ( 'NONE', *, *, #1696, .F. ) ;
#8783 = AXIS2_PLACEMENT_3D ( 'NONE', #9301, #2935, #2829 ) ;
#8784 = ORIENTED_EDGE ( 'NONE', *, *, #7689, .T. ) ;
#8785 = CARTESIAN_POINT ( 'NONE',  ( -7.293506896408097795, 150.5696653505793563, 20.00000000000000355 ) ) ;
#8786 = FACE_OUTER_BOUND ( 'NONE', #7063, .T. ) ;
#8787 = DIRECTION ( 'NONE',  ( 0.000000000000000000, 0.000000000000000000, 1.000000000000000000 ) ) ;
#8788 = DIRECTION ( 'NONE',  ( 0.000000000000000000, 1.000000000000000000, 0.000000000000000000 ) ) ;
#8789 = CARTESIAN_POINT ( 'NONE',  ( -2.293506896408097795, 150.5696653505793563, 0.000000000000000000 ) ) ;
#8790 = EDGE_CURVE ( 'NONE', #10069, #5689, #404, .T. ) ;
#8791 = CIRCLE ( 'NONE', #5059, 4.000000000000000000 ) ;
#8792 = ORIENTED_EDGE ( 'NONE', *, *, #7178, .T. ) ;
#8793 = LINE ( 'NONE', #48, #6031 ) ;
#8794 = ORIENTED_EDGE ( 'NONE', *, *, #691, .F. ) ;
#8795 = CARTESIAN_POINT ( 'NONE',  ( 39.99999999999997158, -145.1457019118819005, 39.99999999999997868 ) ) ;
#8796 = CARTESIAN_POINT ( 'NONE',  ( -93.70792096198771048, 212.3425490925494046, 6.101477040961701944E-16 ) ) ;
#8797 = EDGE_LOOP ( 'NONE', ( #226, #4751, #5548, #8723 ) ) ;
#8798 = PRESENTATION_LAYER_ASSIGNMENT (  '', '', ( #6941 ) ) ;
#8799 = DIRECTION ( 'NONE',  ( 1.000000000000000000, 0.000000000000000000, 0.000000000000000000 ) ) ;
#8800 = CARTESIAN_POINT ( 'NONE',  ( -16.29350689640809691, -8.660287962196477451, -5.025000000000002132 ) ) ;
#8801 = CARTESIAN_POINT ( 'NONE',  ( -142.3328939341254795, 249.4204141414382434, 0.000000000000000000 ) ) ;
#8802 = VERTEX_POINT ( 'NONE', #1935 ) ;
#8803 = ORIENTED_EDGE ( 'NONE', *, *, #8378, .F. ) ;
#8804 = ORIENTED_EDGE ( 'NONE', *, *, #1395, .T. ) ;
#8805 = FACE_OUTER_BOUND ( 'NONE', #6487, .T. ) ;
#8806 = EDGE_CURVE ( 'NONE', #3545, #3742, #3449, .T. ) ;
#8807 = CARTESIAN_POINT ( 'NONE',  ( 39.99999999999997158, -135.1457019118818721, 49.99999999999997868 ) ) ;
#8808 = CARTESIAN_POINT ( 'NONE',  ( -25.28852788137214347, -134.8487249201535008, -50.00000000000002132 ) ) ;
#8809 = FACE_OUTER_BOUND ( 'NONE', #8132, .T. ) ;
#8810 = ORIENTED_EDGE ( 'NONE', *, *, #7749, .T. ) ;
#8811 = DIRECTION ( 'NONE',  ( 0.000000000000000000, 0.000000000000000000, -1.000000000000000000 ) ) ;
#8812 = ORIENTED_EDGE ( 'NONE', *, *, #1786, .T. ) ;
#8813 = AXIS2_PLACEMENT_3D ( 'NONE', #3756, #5235, #3602 ) ;
#8814 = DIRECTION ( 'NONE',  ( 1.000000000000000000, 0.000000000000000000, 0.000000000000000000 ) ) ;
#8815 = PRODUCT ( 'Metal Mounting Block', 'Metal Mounting Block', '', ( #8932 ) ) ;
#8816 = ADVANCED_FACE ( 'NONE', ( #10049 ), #4480, .T. ) ;
#8817 = CARTESIAN_POINT ( 'NONE',  ( -16.29350689640809691, 65.65569765742554864, -4.729641367753004921 ) ) ;
#8818 = DIRECTION ( 'NONE',  ( 0.000000000000000000, -1.000000000000000000, 0.000000000000000000 ) ) ;
#8819 = ORIENTED_EDGE ( 'NONE', *, *, #3498, .F. ) ;
#8820 = COLOUR_RGB ( '',0.7921568627450980005, 0.8196078431372548767, 0.9333333333333333481 ) ;
#8821 = CARTESIAN_POINT ( 'NONE',  ( -30.29350689640809335, 120.5696653505793705, 20.00000000000000711 ) ) ;
#8822 = ORIENTED_EDGE ( 'NONE', *, *, #7256, .T. ) ;
#8823 = CARTESIAN_POINT ( 'NONE',  ( -30.29350689640809335, 50.54838324668256888, -20.00000000000001776 ) ) ;
#8824 = ORIENTED_EDGE ( 'NONE', *, *, #8063, .F. ) ;
#8825 = AXIS2_PLACEMENT_3D ( 'NONE', #3277, #6507, #9755 ) ;
#8826 = CIRCLE ( 'NONE', #1389, 4.000000000000000000 ) ;
#8827 = ORIENTED_EDGE ( 'NONE', *, *, #8699, .F. ) ;
#8828 = EDGE_CURVE ( 'NONE', #2192, #8767, #3796, .T. ) ;
#8829 = EDGE_CURVE ( 'NONE', #2017, #5655, #7023, .T. ) ;
#8830 = DIRECTION ( 'NONE',  ( -1.000000000000000000, 0.000000000000000000, -0.000000000000000000 ) ) ;
#8831 = CARTESIAN_POINT ( 'NONE',  ( -56.36957570605425616, 90.52895752738122326, -10.90000000000000036 ) ) ;
#8832 = DIRECTION ( 'NONE',  ( 0.000000000000000000, -0.4309225046084370070, -0.9023889377768278264 ) ) ;
#8833 = LINE ( 'NONE', #6242, #1546 ) ;
#8834 = DIRECTION ( 'NONE',  ( 0.000000000000000000, 1.000000000000000000, 0.000000000000000000 ) ) ;
#8835 = CIRCLE ( 'NONE', #5454, 1.999999999999998224 ) ;
#8836 = AXIS2_PLACEMENT_3D ( 'NONE', #408, #2731, #5961 ) ;
#8837 = EDGE_LOOP ( 'NONE', ( #10463, #9009 ) ) ;
#8838 = FACE_BOUND ( 'NONE', #9008, .T. ) ;
#8839 = VERTEX_POINT ( 'NONE', #2143 ) ;
#8840 = PRODUCT_RELATED_PRODUCT_CATEGORY ( 'part', '', ( #7892 ) ) ;
#8841 = LINE ( 'NONE', #2968, #2511 ) ;
#8842 = EDGE_CURVE ( 'NONE', #4081, #5556, #4478, .T. ) ;
#8843 = DIRECTION ( 'NONE',  ( 0.000000000000000000, 0.000000000000000000, -1.000000000000000000 ) ) ;
#8844 = ADVANCED_FACE ( 'NONE', ( #3740 ), #4533, .T. ) ;
#8845 = VECTOR ( 'NONE', #7757, 1000.000000000000000 ) ;
#8846 = EDGE_CURVE ( 'NONE', #4224, #9384, #7134, .T. ) ;
#8847 = CIRCLE ( 'NONE', #6284, 7.999999999999994671 ) ;
#8848 = DIRECTION ( 'NONE',  ( -1.000000000000000000, 0.000000000000000000, 0.000000000000000000 ) ) ;
#8849 = CARTESIAN_POINT ( 'NONE',  ( 0.000000000000000000, -145.1457019118819005, 49.99999999999997868 ) ) ;
#8850 = FACE_OUTER_BOUND ( 'NONE', #4332, .T. ) ;
#8851 = ORIENTED_EDGE ( 'NONE', *, *, #7081, .F. ) ;
#8852 = ORIENTED_EDGE ( 'NONE', *, *, #357, .F. ) ;
#8853 = CIRCLE ( 'NONE', #1748, 4.000000000000000000 ) ;
#8854 = ORIENTED_EDGE ( 'NONE', *, *, #317, .T. ) ;
#8855 = CARTESIAN_POINT ( 'NONE',  ( -21.29350689640810046, 105.5289575273812233, -25.04213562373096380 ) ) ;
#8856 = FACE_OUTER_BOUND ( 'NONE', #6779, .T. ) ;
#8857 = EDGE_CURVE ( 'NONE', #1811, #2596, #8612, .T. ) ;
#8858 = CARTESIAN_POINT ( 'NONE',  ( -18.34874108452141783, -140.1746510883711778, -24.43989726270230634 ) ) ;
#8859 = DIRECTION ( 'NONE',  ( -0.7431448254773957984, 0.6691306063588565722, -0.000000000000000000 ) ) ;
#8860 = CIRCLE ( 'NONE', #5637, 2.000000000000001776 ) ;
#8861 = EDGE_LOOP ( 'NONE', ( #6608, #5078, #3674, #7328 ) ) ;
#8862 = LINE ( 'NONE', #5672, #3148 ) ;
#8863 = VERTEX_POINT ( 'NONE', #6332 ) ;
#8864 = FACE_BOUND ( 'NONE', #3262, .T. ) ;
#8865 = EDGE_CURVE ( 'NONE', #2974, #10235, #3904, .T. ) ;
#8866 = TOROIDAL_SURFACE ( 'NONE', #6334, 20.00000000000001776, 4.000000000000000000 ) ;
#8867 = EDGE_LOOP ( 'NONE', ( #2604, #3155, #2733, #1092 ) ) ;
#8868 = ORIENTED_EDGE ( 'NONE', *, *, #4425, .T. ) ;
#8869 = CARTESIAN_POINT ( 'NONE',  ( 37.22511195853868315, -117.1457019118819005, -23.15769640663939910 ) ) ;
#8870 = AXIS2_PLACEMENT_3D ( 'NONE', #4330, #1039, #10163 ) ;
#8871 = DIRECTION ( 'NONE',  ( 0.000000000000000000, 1.000000000000000000, 0.000000000000000000 ) ) ;
#8872 = CARTESIAN_POINT ( 'NONE',  ( -24.31850689640809549, 140.5696653505793563, 20.00000000000002132 ) ) ;
#8873 = EDGE_LOOP ( 'NONE', ( #2074, #2641 ) ) ;
#8874 = CARTESIAN_POINT ( 'NONE',  ( -48.00000000000002842, -117.1457019118819005, 23.15769640663938134 ) ) ;
#8875 = CONTEXT_DEPENDENT_SHAPE_REPRESENTATION ( #712, #1626 ) ;
#8876 = ORIENTED_EDGE ( 'NONE', *, *, #1007, .F. ) ;
#8877 = CARTESIAN_POINT ( 'NONE',  ( 37.22759939293836595, -133.1457019118818721, 25.15769640663938134 ) ) ;
#8878 = VERTEX_POINT ( 'NONE', #3952 ) ;
#8879 = AXIS2_PLACEMENT_3D ( 'NONE', #1076, #6148, #9135 ) ;
#8880 = VERTEX_POINT ( 'NONE', #9410 ) ;
#8881 = DIRECTION ( 'NONE',  ( 0.000000000000000000, 0.000000000000000000, 1.000000000000000000 ) ) ;
#8882 = EDGE_CURVE ( 'NONE', #5001, #9607, #2255, .T. ) ;
#8883 = CIRCLE ( 'NONE', #10249, 3.999999999999989786 ) ;
#8884 = CARTESIAN_POINT ( 'NONE',  ( 25.15769640663936713, -117.1457019118819005, 47.99999999999997868 ) ) ;
#8885 = CARTESIAN_POINT ( 'NONE',  ( 14.70649310359190309, 120.5696653505793705, 20.00000000000000711 ) ) ;
#8886 = CARTESIAN_POINT ( 'NONE',  ( -27.15769640663940976, -117.1457019118819005, 27.15769640663938489 ) ) ;
#8887 = DIRECTION ( 'NONE',  ( -8.194486552889013533E-17, -9.100899318238110877E-17, 1.000000000000000000 ) ) ;
#8888 = ADVANCED_FACE ( 'NONE', ( #5535 ), #7864, .T. ) ;
#8889 = EDGE_CURVE ( 'NONE', #735, #8618, #4637, .T. ) ;
#8890 = ORIENTED_EDGE ( 'NONE', *, *, #1019, .T. ) ;
#8891 = DIRECTION ( 'NONE',  ( -1.000000000000000000, 0.000000000000000000, 0.000000000000000000 ) ) ;
#8892 = EDGE_LOOP ( 'NONE', ( #8719, #1749, #8215, #9447, #8810, #145, #1761, #5570, #8488, #3232, #2687, #2491 ) ) ;
#8893 = CARTESIAN_POINT ( 'NONE',  ( -7.293506896408097795, 126.8146633489777599, 25.00000000000000355 ) ) ;
#8894 = DIRECTION ( 'NONE',  ( 1.000000000000000000, -0.000000000000000000, -0.000000000000000000 ) ) ;
#8895 = FILL_AREA_STYLE ('',( #5758 ) ) ;
#8896 = CARTESIAN_POINT ( 'NONE',  ( -23.76520584195948516, -145.1457019118819005, 49.99999999999997868 ) ) ;
#8897 = CARTESIAN_POINT ( 'NONE',  ( -27.15769640663939555, -115.1457019118818863, -27.15769640663944173 ) ) ;
#8898 = AXIS2_PLACEMENT_3D ( 'NONE', #6551, #1782, #6606 ) ;
#8899 = DIRECTION ( 'NONE',  ( 0.000000000000000000, 0.000000000000000000, 1.000000000000000000 ) ) ;
#8900 = ORIENTED_EDGE ( 'NONE', *, *, #1353, .T. ) ;
#8901 = VERTEX_POINT ( 'NONE', #666 ) ;
#8902 = ADVANCED_FACE ( 'NONE', ( #7871 ), #3098, .T. ) ;
#8903 = EDGE_CURVE ( 'NONE', #5352, #1218, #5028, .T. ) ;
#8904 = ORIENTED_EDGE ( 'NONE', *, *, #9950, .T. ) ;
#8905 = AXIS2_PLACEMENT_3D ( 'NONE', #5072, #5280, #7624 ) ;
#8906 = ADVANCED_FACE ( 'NONE', ( #7183 ), #3794, .F. ) ;
#8907 = PRODUCT_DEFINITION_SHAPE ( 'NONE', 'NONE',  #10490 ) ;
#8908 = VECTOR ( 'NONE', #4313, 1000.000000000000114 ) ;
#8909 = ORIENTED_EDGE ( 'NONE', *, *, #103, .T. ) ;
#8910 = CARTESIAN_POINT ( 'NONE',  ( -2.293506896408097795, 4.007378841484243628E-15, 28.00000000000002132 ) ) ;
#8911 = CYLINDRICAL_SURFACE ( 'NONE', #2575, 7.499999999999998224 ) ;
#8912 = DIRECTION ( 'NONE',  ( 1.000000000000000000, 0.000000000000000000, 0.000000000000000000 ) ) ;
#8913 = AXIS2_PLACEMENT_3D ( 'NONE', #5469, #8057, #801 ) ;
#8914 = ORIENTED_EDGE ( 'NONE', *, *, #8389, .T. ) ;
#8915 = DIRECTION ( 'NONE',  ( -1.000000000000000000, 0.000000000000000000, -0.000000000000000000 ) ) ;
#8916 = AXIS2_PLACEMENT_3D ( 'NONE', #1702, #1655, #7432 ) ;
#8917 = VERTEX_POINT ( 'NONE', #3150 ) ;
#8918 = CARTESIAN_POINT ( 'NONE',  ( -30.29350689640809335, 80.56966535057935630, -16.00000000000000711 ) ) ;
#8919 = EDGE_CURVE ( 'NONE', #9452, #8605, #4140, .T. ) ;
#8920 = CIRCLE ( 'NONE', #4174, 3.999999999999996447 ) ;
#8921 = ORIENTED_EDGE ( 'NONE', *, *, #3538, .T. ) ;
#8922 = ORIENTED_EDGE ( 'NONE', *, *, #7480, .T. ) ;
#8923 = DIRECTION ( 'NONE',  ( 0.000000000000000000, -1.222897680782651471E-16, 1.000000000000000000 ) ) ;
#8924 = AXIS2_PLACEMENT_3D ( 'NONE', #6656, #91, #3317 ) ;
#8925 = DIRECTION ( 'NONE',  ( -0.000000000000000000, 1.000000000000000000, -0.000000000000000000 ) ) ;
#8926 = DIRECTION ( 'NONE',  ( -0.000000000000000000, 0.000000000000000000, -1.000000000000000000 ) ) ;
#8927 = CARTESIAN_POINT ( 'NONE',  ( 17.97972049165455388, 17.84145331825995484, 25.00000000000000000 ) ) ;
#8928 = CIRCLE ( 'NONE', #2662, 4.025000000000000355 ) ;
#8929 = EDGE_LOOP ( 'NONE', ( #1880, #315, #10243, #9558 ) ) ;
#8930 = LINE ( 'NONE', #4106, #1717 ) ;
#8931 = AXIS2_PLACEMENT_3D ( 'NONE', #2067, #10136, #1331 ) ;
#8932 = PRODUCT_CONTEXT ( 'NONE', #3352, 'mechanical' ) ;
#8933 = EDGE_LOOP ( 'NONE', ( #246, #3773 ) ) ;
#8934 = DIRECTION ( 'NONE',  ( -0.000000000000000000, 1.000000000000000000, 0.000000000000000000 ) ) ;
#8935 = ORIENTED_EDGE ( 'NONE', *, *, #4957, .T. ) ;
#8936 = VECTOR ( 'NONE', #390, 1000.000000000000000 ) ;
#8937 = EDGE_CURVE ( 'NONE', #732, #4565, #8201, .T. ) ;
#8938 = FACE_OUTER_BOUND ( 'NONE', #9104, .T. ) ;
#8939 = DIRECTION ( 'NONE',  ( 0.000000000000000000, 1.000000000000000000, 0.000000000000000000 ) ) ;
#8940 = CYLINDRICAL_SURFACE ( 'NONE', #6192, 3.999999999999989786 ) ;
#8941 = FACE_OUTER_BOUND ( 'NONE', #5780, .T. ) ;
#8942 = CYLINDRICAL_SURFACE ( 'NONE', #386, 3.999999999999993339 ) ;
#8943 = AXIS2_PLACEMENT_3D ( 'NONE', #8742, #530, #2333 ) ;
#8944 = ORIENTED_EDGE ( 'NONE', *, *, #4037, .F. ) ;
#8945 = DIRECTION ( 'NONE',  ( 0.000000000000000000, -0.000000000000000000, -1.000000000000000000 ) ) ;
#8946 = AXIS2_PLACEMENT_3D ( 'NONE', #3053, #6282, #7091 ) ;
#8947 = ORIENTED_EDGE ( 'NONE', *, *, #7513, .T. ) ;
#8948 = DIRECTION ( 'NONE',  ( -0.000000000000000000, -0.000000000000000000, 1.000000000000000000 ) ) ;
#8949 = CARTESIAN_POINT ( 'NONE',  ( 0.000000000000000000, 4.898587196589412829E-16, 0.000000000000000000 ) ) ;
#8950 = CYLINDRICAL_SURFACE ( 'NONE', #5735, 2.000000000000001776 ) ;
#8951 = DIRECTION ( 'NONE',  ( 1.000000000000000000, -0.000000000000000000, -0.000000000000000000 ) ) ;
#8952 = EDGE_CURVE ( 'NONE', #7357, #9778, #3250, .T. ) ;
#8953 = DIRECTION ( 'NONE',  ( 0.000000000000000000, 0.000000000000000000, -1.000000000000000000 ) ) ;
#8954 = DIRECTION ( 'NONE',  ( 0.000000000000000000, 0.000000000000000000, -1.000000000000000000 ) ) ;
#8955 = VECTOR ( 'NONE', #2448, 1000.000000000000000 ) ;
#8956 = ORIENTED_EDGE ( 'NONE', *, *, #5872, .F. ) ;
#8957 = EDGE_LOOP ( 'NONE', ( #9421, #7821, #2329, #2909, #3618, #8475, #5274, #962, #7025, #9328, #7610, #5325, #4370 ) ) ;
#8958 = VERTEX_POINT ( 'NONE', #4837 ) ;
#8959 = ORIENTED_EDGE ( 'NONE', *, *, #4829, .F. ) ;
#8960 = AXIS2_PLACEMENT_3D ( 'NONE', #7360, #9811, #162 ) ;
#8961 = PLANE ( 'NONE',  #4865 ) ;
#8962 = SURFACE_STYLE_FILL_AREA ( #8111 ) ;
#8963 = ORIENTED_EDGE ( 'NONE', *, *, #9237, .F. ) ;
#8964 = CARTESIAN_POINT ( 'NONE',  ( -30.29350689640809335, 120.5696653505793705, -16.00000000000000711 ) ) ;
#8965 = EDGE_CURVE ( 'NONE', #2439, #2209, #4975, .T. ) ;
#8966 = CARTESIAN_POINT ( 'NONE',  ( 14.70649310359190309, 80.56966535057935630, 20.00000000000000711 ) ) ;
#8967 = EDGE_CURVE ( 'NONE', #7130, #6316, #7355, .T. ) ;
#8968 = EDGE_CURVE ( 'NONE', #8878, #7051, #6427, .T. ) ;
#8969 = VERTEX_POINT ( 'NONE', #8817 ) ;
#8970 = CARTESIAN_POINT ( 'NONE',  ( -122.5292777575814114, 231.5891580443559121, 0.000000000000000000 ) ) ;
#8971 = EDGE_LOOP ( 'NONE', ( #4555, #4212, #7453, #6174 ) ) ;
#8972 = VERTEX_POINT ( 'NONE', #8019 ) ;
#8973 = UNCERTAINTY_MEASURE_WITH_UNIT (LENGTH_MEASURE( 1.000000000000000082E-05 ), #7876, 'distance_accuracy_value', 'NONE');
#8974 = LINE ( 'NONE', #9130, #129 ) ;
#8975 = SURFACE_STYLE_FILL_AREA ( #2664 ) ;
#8976 = CARTESIAN_POINT ( 'NONE',  ( 59.99999999999997868, -135.1457019118818721, 40.00000000000000000 ) ) ;
#8977 = CYLINDRICAL_SURFACE ( 'NONE', #6124, 2.000000000000001776 ) ;
#8978 = EDGE_CURVE ( 'NONE', #2082, #1644, #9573, .T. ) ;
#8979 = ADVANCED_FACE ( 'NONE', ( #4991, #2512 ), #187, .T. ) ;
#8980 = EDGE_CURVE ( 'NONE', #7171, #8802, #8709, .T. ) ;
#8981 = LINE ( 'NONE', #7388, #8542 ) ;
#8982 = DIRECTION ( 'NONE',  ( -0.000000000000000000, -0.000000000000000000, -1.000000000000000000 ) ) ;
#8983 = VERTEX_POINT ( 'NONE', #862 ) ;
#8984 = CYLINDRICAL_SURFACE ( 'NONE', #864, 3.999999999999989786 ) ;
#8985 = ORIENTED_EDGE ( 'NONE', *, *, #9751, .T. ) ;
#8986 = CARTESIAN_POINT ( 'NONE',  ( -25.28853996896956957, -134.8487302617674857, 49.99999999999998579 ) ) ;
#8987 = ORIENTED_EDGE ( 'NONE', *, *, #9438, .F. ) ;
#8988 = SPHERICAL_SURFACE ( 'NONE', #9614, 2.000000000000000000 ) ;
#8989 = AXIS2_PLACEMENT_3D ( 'NONE', #9485, #5496, #7102 ) ;
#8990 = DIRECTION ( 'NONE',  ( 0.000000000000000000, 0.7071067811864494290, 0.7071067811866454944 ) ) ;
#8991 = CARTESIAN_POINT ( 'NONE',  ( 4.856471286862175774, 152.5696653505793279, 30.00000000000000355 ) ) ;
#8992 = FILL_AREA_STYLE_COLOUR ( '', #2719 ) ;
#8993 = DIRECTION ( 'NONE',  ( -0.000000000000000000, 1.000000000000000000, -0.000000000000000000 ) ) ;
#8994 = EDGE_CURVE ( 'NONE', #5189, #4587, #9048, .T. ) ;
#8995 = ORIENTED_EDGE ( 'NONE', *, *, #4801, .T. ) ;
#8996 = DIRECTION ( 'NONE',  ( 0.000000000000000000, 1.000000000000000000, 0.000000000000000000 ) ) ;
#8997 = AXIS2_PLACEMENT_3D ( 'NONE', #7599, #1969, #1918 ) ;
#8998 = ORIENTED_EDGE ( 'NONE', *, *, #9679, .T. ) ;
#8999 = DIRECTION ( 'NONE',  ( -0.000000000000000000, -1.000000000000000000, -0.000000000000000000 ) ) ;
#9000 = CARTESIAN_POINT ( 'NONE',  ( 37.59878849545336976, 32.08684478514406635, -12.49999999999999289 ) ) ;
#9001 = ORIENTED_EDGE ( 'NONE', *, *, #3597, .F. ) ;
#9002 = LINE ( 'NONE', #8148, #235 ) ;
#9003 = CARTESIAN_POINT ( 'NONE',  ( -2.293506896408097795, 72.08684478514406635, 28.00000000000001066 ) ) ;
#9004 = CIRCLE ( 'NONE', #4101, 4.000000000000000000 ) ;
#9005 = DIRECTION ( 'NONE',  ( -0.000000000000000000, 0.000000000000000000, 1.000000000000000000 ) ) ;
#9006 = VECTOR ( 'NONE', #9618, 1000.000000000000227 ) ;
#9007 = SHAPE_REPRESENTATION ( 'MAS-316', ( #584, #8870, #4962, #5815, #4300, #7685, #2094, #2606, #4641, #9038, #917, #10234, #9727 ), #5145 ) ;
#9008 = EDGE_LOOP ( 'NONE', ( #4409, #4667 ) ) ;
#9009 = ORIENTED_EDGE ( 'NONE', *, *, #8390, .F. ) ;
#9010 = EDGE_CURVE ( 'NONE', #596, #3403, #10241, .T. ) ;
#9011 = CIRCLE ( 'NONE', #214, 2.541999999999999815 ) ;
#9012 = ORIENTED_EDGE ( 'NONE', *, *, #2153, .T. ) ;
#9013 = CARTESIAN_POINT ( 'NONE',  ( 3.000000000000000000, -1.467624384280024730, 2.542000000000003368 ) ) ;
#9014 = CARTESIAN_POINT ( 'NONE',  ( 23.15769640663936713, -117.1457019118819005, 47.99999999999997868 ) ) ;
#9015 = DIRECTION ( 'NONE',  ( 0.000000000000000000, 0.000000000000000000, -1.000000000000000000 ) ) ;
#9016 = LINE ( 'NONE', #2602, #5207 ) ;
#9017 = ORIENTED_EDGE ( 'NONE', *, *, #371, .F. ) ;
#9018 = DIRECTION ( 'NONE',  ( 0.000000000000000000, 0.000000000000000000, -1.000000000000000000 ) ) ;
#9019 = AXIS2_PLACEMENT_3D ( 'NONE', #4470, #1287, #10037 ) ;
#9020 = ORIENTED_EDGE ( 'NONE', *, *, #1787, .F. ) ;
#9021 = CARTESIAN_POINT ( 'NONE',  ( -7.293506896408097795, -0.3998014571812398832, -1.076388538564875708 ) ) ;
#9022 = EDGE_CURVE ( 'NONE', #8802, #7171, #83, .T. ) ;
#9023 = VERTEX_POINT ( 'NONE', #5633 ) ;
#9024 = ORIENTED_EDGE ( 'NONE', *, *, #1456, .T. ) ;
#9025 = FACE_OUTER_BOUND ( 'NONE', #8631, .T. ) ;
#9026 = FACE_BOUND ( 'NONE', #8933, .T. ) ;
#9027 = AXIS2_PLACEMENT_3D ( 'NONE', #6305, #9496, #4718 ) ;
#9028 = CARTESIAN_POINT ( 'NONE',  ( -50.00000000000002132, -117.1457019118819005, 23.15769640663938134 ) ) ;
#9029 = CARTESIAN_POINT ( 'NONE',  ( -40.00000000000002842, -135.1457019118818721, 44.02499999999997726 ) ) ;
#9030 = CARTESIAN_POINT ( 'NONE',  ( -16.29350689640809691, -8.660287962196477451, 0.000000000000000000 ) ) ;
#9031 = DIRECTION ( 'NONE',  ( 0.000000000000000000, 0.000000000000000000, -1.000000000000000000 ) ) ;
#9032 = ORIENTED_EDGE ( 'NONE', *, *, #5653, .F. ) ;
#9033 = DIRECTION ( 'NONE',  ( 0.000000000000000000, 0.000000000000000000, -1.000000000000000000 ) ) ;
#9034 = AXIS2_PLACEMENT_3D ( 'NONE', #4495, #1895, #6938 ) ;
#9035 = EDGE_CURVE ( 'NONE', #109, #1323, #8022, .T. ) ;
#9037 = EDGE_CURVE ( 'NONE', #2663, #2288, #8981, .T. ) ;
#9036 = ORIENTED_EDGE ( 'NONE', *, *, #6169, .T. ) ;
#9038 = AXIS2_PLACEMENT_3D ( 'NONE', #8667, #9636, #3856 ) ;
#9039 = ADVANCED_FACE ( 'NONE', ( #818 ), #2455, .F. ) ;
#9040 = CARTESIAN_POINT ( 'NONE',  ( 4.467624384280048488, 0.000000000000000000, 0.000000000000000000 ) ) ;
#9041 = ORIENTED_EDGE ( 'NONE', *, *, #2443, .T. ) ;
#9042 = AXIS2_PLACEMENT_3D ( 'NONE', #8296, #6010, #1089 ) ;
#9043 = CARTESIAN_POINT ( 'NONE',  ( 25.15769640663938134, -135.1457019118818721, -27.15769640663941331 ) ) ;
#9044 = PLANE ( 'NONE',  #1082 ) ;
#9045 = DIRECTION ( 'NONE',  ( 8.659560562355001884E-17, 0.7071067811865420216, -0.7071067811865531239 ) ) ;
#9046 = DIRECTION ( 'NONE',  ( -1.000000000000000000, -0.000000000000000000, 0.000000000000000000 ) ) ;
#9047 = ORIENTED_EDGE ( 'NONE', *, *, #4646, .T. ) ;
#9048 = CIRCLE ( 'NONE', #3805, 4.025000000000000355 ) ;
#9049 = EDGE_CURVE ( 'NONE', #1535, #8552, #1610, .T. ) ;
#9050 = CARTESIAN_POINT ( 'NONE',  ( -30.29350689640809335, 2.445795361565304815E-15, 20.00000000000002132 ) ) ;
#9051 = ORIENTED_EDGE ( 'NONE', *, *, #1324, .F. ) ;
#9052 = DIRECTION ( 'NONE',  ( 0.000000000000000000, -0.5150380749100554878, -0.8571673007021115565 ) ) ;
#9053 = DIRECTION ( 'NONE',  ( 0.000000000000000000, -0.000000000000000000, 1.000000000000000000 ) ) ;
#9054 = CARTESIAN_POINT ( 'NONE',  ( -93.80004353141508489, 205.7212393575359783, 0.000000000000000000 ) ) ;
#9055 = CARTESIAN_POINT ( 'NONE',  ( -16.29350689640809691, -8.660287962196477451, -7.499999999999998224 ) ) ;
#9056 = CARTESIAN_POINT ( 'NONE',  ( 39.99999999999998579, -145.1457019118819005, -40.00000000000002132 ) ) ;
#9057 = VECTOR ( 'NONE', #3060, 1000.000000000000114 ) ;
#9058 = EDGE_LOOP ( 'NONE', ( #6577, #3299 ) ) ;
#9059 = VERTEX_POINT ( 'NONE', #4890 ) ;
#9060 = ORIENTED_EDGE ( 'NONE', *, *, #8857, .F. ) ;
#9061 = LINE ( 'NONE', #9714, #1320 ) ;
#9062 = AXIS2_PLACEMENT_3D ( 'NONE', #2634, #5750, #8248 ) ;
#9063 = DIRECTION ( 'NONE',  ( 0.000000000000000000, 0.000000000000000000, 1.000000000000000000 ) ) ;
#9064 = EDGE_CURVE ( 'NONE', #7484, #3453, #2951, .T. ) ;
#9065 = CARTESIAN_POINT ( 'NONE',  ( -39.00428932080996702, -3.065011249696382389, -1.804608920635915492 ) ) ;
#9066 = ORIENTED_EDGE ( 'NONE', *, *, #356, .T. ) ;
#9067 = DIRECTION ( 'NONE',  ( 0.000000000000000000, 1.000000000000000000, 0.000000000000000000 ) ) ;
#9068 = AXIS2_PLACEMENT_3D ( 'NONE', #10223, #2953, #7040 ) ;
#9069 = ORIENTED_EDGE ( 'NONE', *, *, #6556, .T. ) ;
#9070 = DIRECTION ( 'NONE',  ( 1.000000000000000000, 0.000000000000000000, -0.000000000000000000 ) ) ;
#9071 = AXIS2_PLACEMENT_3D ( 'NONE', #2565, #4211, #7337 ) ;
#9072 = ORIENTED_EDGE ( 'NONE', *, *, #5784, .T. ) ;
#9073 = UNCERTAINTY_MEASURE_WITH_UNIT (LENGTH_MEASURE( 1.000000000000000082E-05 ), #3530, 'distance_accuracy_value', 'NONE');
#9074 = LINE ( 'NONE', #8282, #3005 ) ;
#9075 = DIRECTION ( 'NONE',  ( -1.000000000000000000, 0.000000000000000000, 0.000000000000000000 ) ) ;
#9076 = AXIS2_PLACEMENT_3D ( 'NONE', #2059, #8532, #1270 ) ;
#9077 = CARTESIAN_POINT ( 'NONE',  ( 59.99999999999999289, -135.1457019118818721, -40.00000000000000000 ) ) ;
#9078 = CARTESIAN_POINT ( 'NONE',  ( 39.99999999999997158, -145.1457019118819005, 39.99999999999997868 ) ) ;
#9079 = AXIS2_PLACEMENT_3D ( 'NONE', #10434, #8682, #6397 ) ;
#9080 = CARTESIAN_POINT ( 'NONE',  ( -30.29350689640809335, 80.56966535057935630, -28.00000000000000355 ) ) ;
#9081 = ADVANCED_FACE ( 'NONE', ( #6593 ), #9840, .F. ) ;
#9082 = CARTESIAN_POINT ( 'NONE',  ( 18.34874108452142494, -140.1746510883711778, -50.00000000000002132 ) ) ;
#9083 = VERTEX_POINT ( 'NONE', #6646 ) ;
#9084 = DIRECTION ( 'NONE',  ( 0.000000000000000000, -0.000000000000000000, 1.000000000000000000 ) ) ;
#9085 = AXIS2_PLACEMENT_3D ( 'NONE', #5651, #685, #3922 ) ;
#9086 = ORIENTED_EDGE ( 'NONE', *, *, #5142, .T. ) ;
#9087 = CARTESIAN_POINT ( 'NONE',  ( -23.15769640663940976, -133.1457019118818721, 49.99999999999997868 ) ) ;
#9088 = VERTEX_POINT ( 'NONE', #5583 ) ;
#9089 =( NAMED_UNIT ( * ) SI_UNIT ( $, .STERADIAN. ) SOLID_ANGLE_UNIT ( ) );
#9090 = ORIENTED_EDGE ( 'NONE', *, *, #8806, .F. ) ;
#9091 = VECTOR ( 'NONE', #7763, 1000.000000000000000 ) ;
#9092 = DIRECTION ( 'NONE',  ( 7.848480207562752404E-17, 1.000000000000000000, -8.929448294704472850E-33 ) ) ;
#9093 = DIRECTION ( 'NONE',  ( 0.000000000000000000, 0.000000000000000000, 1.000000000000000000 ) ) ;
#9094 = EDGE_CURVE ( 'NONE', #6578, #2209, #5318, .T. ) ;
#9095 = ADVANCED_FACE ( 'NONE', ( #8287 ), #5313, .T. ) ;
#9096 = PLANE ( 'NONE',  #1957 ) ;
#9097 = EDGE_CURVE ( 'NONE', #7666, #5994, #6673, .T. ) ;
#9098 = CYLINDRICAL_SURFACE ( 'NONE', #859, 7.999999999999994671 ) ;
#9099 = AXIS2_PLACEMENT_3D ( 'NONE', #6147, #5193, #8430 ) ;
#9100 = CARTESIAN_POINT ( 'NONE',  ( -18.34874108452141783, -140.1746510883711778, 24.43989726270226370 ) ) ;
#9101 = ORIENTED_EDGE ( 'NONE', *, *, #7195, .F. ) ;
#9102 = AXIS2_PLACEMENT_3D ( 'NONE', #6317, #9666, #9617 ) ;
#9103 = DIRECTION ( 'NONE',  ( 0.6691306063588561281, 0.7431448254773961315, 0.000000000000000000 ) ) ;
#9104 = EDGE_LOOP ( 'NONE', ( #5822, #7237, #1544, #9782 ) ) ;
#9105 = CARTESIAN_POINT ( 'NONE',  ( -16.29350689640809691, -115.1457019118818863, -23.72119897386845722 ) ) ;
#9106 = CARTESIAN_POINT ( 'NONE',  ( -23.15769640663940265, -117.1457019118819005, -3.234176690190487260E-15 ) ) ;
#9107 = DIRECTION ( 'NONE',  ( -1.000000000000000000, 0.000000000000000000, 0.000000000000000000 ) ) ;
#9108 = CARTESIAN_POINT ( 'NONE',  ( -47.94539818030330025, 150.5696653505793563, 0.000000000000000000 ) ) ;
#9109 = FACE_OUTER_BOUND ( 'NONE', #7265, .T. ) ;
#9110 = AXIS2_PLACEMENT_3D ( 'NONE', #3878, #10343, #3928 ) ;
#9111 = ADVANCED_FACE ( 'NONE', ( #4258 ), #4803, .F. ) ;
#9112 = CYLINDRICAL_SURFACE ( 'NONE', #9392, 2.000000000000001776 ) ;
#9113 = CIRCLE ( 'NONE', #2180, 7.999999999999996447 ) ;
#9114 = VERTEX_POINT ( 'NONE', #4312 ) ;
#9115 = VECTOR ( 'NONE', #8999, 1000.000000000000000 ) ;
#9116 = ORIENTED_EDGE ( 'NONE', *, *, #5858, .F. ) ;
#9117 = ORIENTED_EDGE ( 'NONE', *, *, #1976, .T. ) ;
#9118 = DIRECTION ( 'NONE',  ( 0.000000000000000000, 0.000000000000000000, 1.000000000000000000 ) ) ;
#9119 = DIRECTION ( 'NONE',  ( 1.000000000000000000, 0.000000000000000000, 0.000000000000000000 ) ) ;
#9120 = AXIS2_PLACEMENT_3D ( 'NONE', #4146, #8170, #10461 ) ;
#9121 = DIRECTION ( 'NONE',  ( -0.7071067811865431318, 0.000000000000000000, 0.7071067811865520136 ) ) ;
#9122 = DIRECTION ( 'NONE',  ( 0.000000000000000000, 0.000000000000000000, -1.000000000000000000 ) ) ;
#9123 = ORIENTED_EDGE ( 'NONE', *, *, #2111, .T. ) ;
#9124 = LINE ( 'NONE', #2705, #3845 ) ;
#9125 = VERTEX_POINT ( 'NONE', #7745 ) ;
#9126 = DIRECTION ( 'NONE',  ( 0.000000000000000000, 0.000000000000000000, 1.000000000000000000 ) ) ;
#9127 = CIRCLE ( 'NONE', #3552, 2.541999999999999815 ) ;
#9128 = ADVANCED_FACE ( 'NONE', ( #8591, #3519 ), #4560, .T. ) ;
#9129 = ORIENTED_EDGE ( 'NONE', *, *, #10002, .F. ) ;
#9130 = CARTESIAN_POINT ( 'NONE',  ( -23.15769640663940976, -115.1457019118818863, -1.617088345095243827E-14 ) ) ;
#9131 = CARTESIAN_POINT ( 'NONE',  ( -56.36957570605427037, 137.0132282531173473, -3.999999999999989786 ) ) ;
#9132 = LINE ( 'NONE', #8177, #6871 ) ;
#9133 = DIRECTION ( 'NONE',  ( 1.000000000000000000, 0.000000000000000000, 0.000000000000000000 ) ) ;
#9134 = VECTOR ( 'NONE', #8522, 1000.000000000000000 ) ;
#9135 = DIRECTION ( 'NONE',  ( 0.000000000000000000, 0.5000000000000011102, 0.8660254037844379305 ) ) ;
#9136 = CARTESIAN_POINT ( 'NONE',  ( 37.23187270759618883, -133.8059336968422883, -25.26512318821856340 ) ) ;
#9137 = ORIENTED_EDGE ( 'NONE', *, *, #430, .F. ) ;
#9138 = CARTESIAN_POINT ( 'NONE',  ( -38.96131932220313132, 3.592756407884963199, -1.758437202063674487 ) ) ;
#9139 = ORIENTED_EDGE ( 'NONE', *, *, #1306, .F. ) ;
#9140 = FACE_OUTER_BOUND ( 'NONE', #3830, .T. ) ;
#9141 = ADVANCED_FACE ( 'NONE', ( #7545, #2918 ), #5154, .F. ) ;
#9142 = ORIENTED_EDGE ( 'NONE', *, *, #9653, .T. ) ;
#9143 = CARTESIAN_POINT ( 'NONE',  ( 39.99999999999998579, -145.1457019118819005, -40.00000000000002132 ) ) ;
#9144 = DIRECTION ( 'NONE',  ( 0.000000000000000000, 0.4999999999999985012, -0.8660254037844393737 ) ) ;
#9145 = LINE ( 'NONE', #1885, #2308 ) ;
#9146 = ORIENTED_EDGE ( 'NONE', *, *, #5478, .F. ) ;
#9147 = DIRECTION ( 'NONE',  ( 0.000000000000000000, 0.000000000000000000, 1.000000000000000000 ) ) ;
#9148 = DIRECTION ( 'NONE',  ( 0.000000000000000000, 0.000000000000000000, 1.000000000000000000 ) ) ;
#9149 = ORIENTED_EDGE ( 'NONE', *, *, #10385, .T. ) ;
#9150 = CARTESIAN_POINT ( 'NONE',  ( -47.94539818030330025, 150.5696653505793563, 0.000000000000000000 ) ) ;
#9151 = EDGE_CURVE ( 'NONE', #9794, #7113, #1332, .T. ) ;
#9152 = ADVANCED_FACE ( 'NONE', ( #9946 ), #7847, .F. ) ;
#9153 = AXIS2_PLACEMENT_3D ( 'NONE', #8886, #2525, #8138 ) ;
#9154 = ORIENTED_EDGE ( 'NONE', *, *, #8378, .T. ) ;
#9155 = DIRECTION ( 'NONE',  ( 0.000000000000000000, 0.000000000000000000, 1.000000000000000000 ) ) ;
#9156 = CARTESIAN_POINT ( 'NONE',  ( -2.293506896408097795, 37.08684478514406635, 30.00000000000000355 ) ) ;
#9157 = DIRECTION ( 'NONE',  ( 0.000000000000000000, -1.000000000000000000, 0.000000000000000000 ) ) ;
#9158 = CARTESIAN_POINT ( 'NONE',  ( -1.071796769724492338, -3.592756407884937442, -1.758437202063728222 ) ) ;
#9159 = CARTESIAN_POINT ( 'NONE',  ( 39.99999999999997158, -135.1457019118818721, 39.99999999999997868 ) ) ;
#9160 = DIRECTION ( 'NONE',  ( -1.000000000000000000, -0.000000000000000000, -8.379529552680125332E-16 ) ) ;
#9161 = AXIS2_PLACEMENT_3D ( 'NONE', #1508, #8655, #10410 ) ;
#9162 = VERTEX_POINT ( 'NONE', #4511 ) ;
#9163=STYLED_ITEM('',(#10525),#9837);
#9164 = ORIENTED_EDGE ( 'NONE', *, *, #4724, .F. ) ;
#9165 = EDGE_CURVE ( 'NONE', #3261, #5755, #6501, .T. ) ;
#9166 = ADVANCED_FACE ( 'NONE', ( #5943 ), #2668, .T. ) ;
#9167 = ADVANCED_FACE ( 'NONE', ( #5841 ), #9389, .F. ) ;
#9168 = DIRECTION ( 'NONE',  ( -1.000000000000000000, 0.000000000000000000, 0.000000000000000000 ) ) ;
#9169 = PLANE ( 'NONE',  #3590 ) ;
#9170 = VECTOR ( 'NONE', #7128, 1000.000000000000000 ) ;
#9171 =( GEOMETRIC_REPRESENTATION_CONTEXT ( 3 ) GLOBAL_UNCERTAINTY_ASSIGNED_CONTEXT ( ( #75 ) ) GLOBAL_UNIT_ASSIGNED_CONTEXT ( ( #6894, #10132, #9981 ) ) REPRESENTATION_CONTEXT ( 'NONE', 'WORKASPACE' ) );
#9172 = CARTESIAN_POINT ( 'NONE',  ( -7.293506896408098683, 145.5696653505793563, 20.00000000000000711 ) ) ;
#9173 = LINE ( 'NONE', #1062, #1818 ) ;
#9174 = ORIENTED_EDGE ( 'NONE', *, *, #4771, .T. ) ;
#9175 = FACE_OUTER_BOUND ( 'NONE', #696, .T. ) ;
#9176 = VERTEX_POINT ( 'NONE', #1871 ) ;
#9177 = CYLINDRICAL_SURFACE ( 'NONE', #4889, 4.000000000000000000 ) ;
#9178 = CIRCLE ( 'NONE', #6634, 2.000000000000001776 ) ;
#9179 = AXIS2_PLACEMENT_3D ( 'NONE', #6280, #9635, #5484 ) ;
#9180 = VERTEX_POINT ( 'NONE', #10185 ) ;
#9181 = EDGE_CURVE ( 'NONE', #1695, #6356, #3771, .T. ) ;
#9182 = ORIENTED_EDGE ( 'NONE', *, *, #1200, .T. ) ;
#9183 = PLANE ( 'NONE',  #5710 ) ;
#9184 = FACE_OUTER_BOUND ( 'NONE', #10040, .T. ) ;
#9185 = FACE_OUTER_BOUND ( 'NONE', #1231, .T. ) ;
#9186 = CARTESIAN_POINT ( 'NONE',  ( -16.29350689640809691, -140.1746510883711778, 0.000000000000000000 ) ) ;
#9187 = VECTOR ( 'NONE', #7647, 1000.000000000000000 ) ;
#9188 = AXIS2_PLACEMENT_3D ( 'NONE', #7076, #3041, #5475 ) ;
#9189 = DIRECTION ( 'NONE',  ( 0.000000000000000000, 0.000000000000000000, 1.000000000000000000 ) ) ;
#9190 = EDGE_CURVE ( 'NONE', #8878, #7930, #6203, .T. ) ;
#9191 = CARTESIAN_POINT ( 'NONE',  ( -16.29350689640809691, 105.5289575273812233, -7.750000000000000000 ) ) ;
#9192 = ORIENTED_EDGE ( 'NONE', *, *, #5596, .F. ) ;
#9193 = CARTESIAN_POINT ( 'NONE',  ( 4.856471286862175774, 147.5696653505793279, -30.00000000000000355 ) ) ;
#9194 = ORIENTED_EDGE ( 'NONE', *, *, #2895, .T. ) ;
#9195 = VECTOR ( 'NONE', #6256, 1000.000000000000000 ) ;
#9196 = CYLINDRICAL_SURFACE ( 'NONE', #7104, 2.000000000000001776 ) ;
#9197 = ORIENTED_EDGE ( 'NONE', *, *, #6366, .T. ) ;
#9198 = DIRECTION ( 'NONE',  ( 0.000000000000000000, 0.000000000000000000, 1.000000000000000000 ) ) ;
#9199 = CARTESIAN_POINT ( 'NONE',  ( -39.00436953563450970, 0.03089877619826473382, 3.555871974361681342 ) ) ;
#9200 = ADVANCED_FACE ( 'NONE', ( #8638 ), #4612, .T. ) ;
#9201 = CARTESIAN_POINT ( 'NONE',  ( -8.000000000000000000, -0.1799657291978226659, -2.057017697435776338 ) ) ;
#9202 = VERTEX_POINT ( 'NONE', #6259 ) ;
#9203 = LINE ( 'NONE', #1993, #4938 ) ;
#9204 = AXIS2_PLACEMENT_3D ( 'NONE', #3072, #4029, #2228 ) ;
#9205 = ORIENTED_EDGE ( 'NONE', *, *, #7956, .F. ) ;
#9206 = DIRECTION ( 'NONE',  ( 0.000000000000000000, 0.000000000000000000, -1.000000000000000000 ) ) ;
#9207 = ORIENTED_EDGE ( 'NONE', *, *, #6642, .T. ) ;
#9208 = CARTESIAN_POINT ( 'NONE',  ( -38.19229777560033057, 152.5696653505793279, 12.50000000000000000 ) ) ;
#9209 = AXIS2_PLACEMENT_3D ( 'NONE', #877, #1621, #4899 ) ;
#9210 = ADVANCED_FACE ( 'NONE', ( #647 ), #9224, .F. ) ;
#9211 = EDGE_LOOP ( 'NONE', ( #1227, #6988, #4897, #3442 ) ) ;
#9212 = SPHERICAL_SURFACE ( 'NONE', #282, 2.000000000000000000 ) ;
#9213 = CARTESIAN_POINT ( 'NONE',  ( 99.80027788547049283, -145.1457019118819005, -24.99999999999998934 ) ) ;
#9214 =( GEOMETRIC_REPRESENTATION_CONTEXT ( 3 ) GLOBAL_UNCERTAINTY_ASSIGNED_CONTEXT ( ( #1762 ) ) GLOBAL_UNIT_ASSIGNED_CONTEXT ( ( #9279, #1956, #4321 ) ) REPRESENTATION_CONTEXT ( 'NONE', 'WORKASPACE' ) );
#9215 = PLANE ( 'NONE',  #1 ) ;
#9216 = CARTESIAN_POINT ( 'NONE',  ( 33.55285093437175448, 29.14909237014566301, -12.50000000000000000 ) ) ;
#9217 = FACE_OUTER_BOUND ( 'NONE', #10212, .T. ) ;
#9218 = DIRECTION ( 'NONE',  ( 0.000000000000000000, 0.000000000000000000, 1.000000000000000000 ) ) ;
#9219 = ADVANCED_FACE ( 'NONE', ( #8047 ), #3885, .T. ) ;
#9220 = AXIS2_PLACEMENT_3D ( 'NONE', #761, #7234, #6482 ) ;
#9221 = ORIENTED_EDGE ( 'NONE', *, *, #2845, .F. ) ;
#9222 = ORIENTED_EDGE ( 'NONE', *, *, #4942, .F. ) ;
#9223 = CARTESIAN_POINT ( 'NONE',  ( -3.173844575093148990, 150.5696653505793563, 10.90000000000000036 ) ) ;
#9224 = TOROIDAL_SURFACE ( 'NONE', #3132, 3.250000000000000444, 0.2500000000000000000 ) ;
#9225 = LINE ( 'NONE', #8536, #4118 ) ;
#9226 = DIRECTION ( 'NONE',  ( 0.000000000000000000, -1.000000000000000000, 0.000000000000000000 ) ) ;
#9227 = ORIENTED_EDGE ( 'NONE', *, *, #964, .F. ) ;
#9228 = EDGE_CURVE ( 'NONE', #3945, #2288, #7528, .T. ) ;
#9229 = DIRECTION ( 'NONE',  ( 0.000000000000000000, -1.000000000000000000, -9.100899318238115807E-17 ) ) ;
#9230 = ADVANCED_FACE ( 'NONE', ( #8748 ), #6360, .F. ) ;
#9231 = ADVANCED_FACE ( 'NONE', ( #3931 ), #2113, .T. ) ;
#9232 = ORIENTED_EDGE ( 'NONE', *, *, #4696, .F. ) ;
#9233 = DIRECTION ( 'NONE',  ( 0.000000000000000000, 0.000000000000000000, 1.000000000000000000 ) ) ;
#9234 = ORIENTED_EDGE ( 'NONE', *, *, #6086, .T. ) ;
#9235 = LINE ( 'NONE', #10034, #5547 ) ;
#9236 = CARTESIAN_POINT ( 'NONE',  ( -30.29350689640809335, 2.445795361565304815E-15, -20.00000000000002132 ) ) ;
#9237 = EDGE_CURVE ( 'NONE', #6945, #3843, #8001, .T. ) ;
#9238 = FACE_OUTER_BOUND ( 'NONE', #8867, .T. ) ;
#9239 = DIRECTION ( 'NONE',  ( 0.000000000000000000, 0.000000000000000000, -1.000000000000000000 ) ) ;
#9240 = AXIS2_PLACEMENT_3D ( 'NONE', #6640, #7600, #3303 ) ;
#9241 = DIRECTION ( 'NONE',  ( -0.6691306063588561281, -0.7431448254773960205, 0.000000000000000000 ) ) ;
#9242 = CIRCLE ( 'NONE', #2464, 3.999999999999976019 ) ;
#9243 = ADVANCED_FACE ( 'NONE', ( #8850 ), #3074, .T. ) ;
#9244 = ORIENTED_EDGE ( 'NONE', *, *, #7278, .F. ) ;
#9245 = DIRECTION ( 'NONE',  ( 0.000000000000000000, 0.000000000000000000, -1.000000000000000000 ) ) ;
#9246 = ORIENTED_EDGE ( 'NONE', *, *, #8968, .T. ) ;
#9247 = AXIS2_PLACEMENT_3D ( 'NONE', #3679, #4622, #2766 ) ;
#9248 = DIRECTION ( 'NONE',  ( -0.000000000000000000, -0.000000000000000000, 1.000000000000000000 ) ) ;
#9249 = FACE_OUTER_BOUND ( 'NONE', #1694, .T. ) ;
#9250 = CIRCLE ( 'NONE', #10100, 19.24539146688411506 ) ;
#9251 = DIRECTION ( 'NONE',  ( 0.000000000000000000, 0.000000000000000000, 1.000000000000000000 ) ) ;
#9252 = DIRECTION ( 'NONE',  ( -1.000000000000000000, -0.000000000000000000, -0.000000000000000000 ) ) ;
#9253 = DIRECTION ( 'NONE',  ( -0.000000000000000000, 0.000000000000000000, -1.000000000000000000 ) ) ;
#9254 = CARTESIAN_POINT ( 'NONE',  ( -16.29350689640809691, -8.660287962196477451, 0.000000000000000000 ) ) ;
#9255 = ORIENTED_EDGE ( 'NONE', *, *, #8736, .F. ) ;
#9256 = FACE_OUTER_BOUND ( 'NONE', #9634, .T. ) ;
#9257 = TOROIDAL_SURFACE ( 'NONE', #6721, 4.700000000000000178, 0.2999999999999999889 ) ;
#9258 = ORIENTED_EDGE ( 'NONE', *, *, #9817, .T. ) ;
#9259 = EDGE_LOOP ( 'NONE', ( #3310, #6239, #9354, #6778 ) ) ;
#9260 = CARTESIAN_POINT ( 'NONE',  ( -16.29350689640809691, 88.12362273389504708, 0.000000000000000000 ) ) ;
#9261 = EDGE_CURVE ( 'NONE', #8972, #426, #2286, .T. ) ;
#9262 = TOROIDAL_SURFACE ( 'NONE', #10455, 4.000000000000000000, 2.000000000000000000 ) ;
#9263 = VERTEX_POINT ( 'NONE', #740 ) ;
#9264 = CARTESIAN_POINT ( 'NONE',  ( -23.17384457509314899, 130.5696653505793847, -10.90000000000000036 ) ) ;
#9265 = DIRECTION ( 'NONE',  ( 0.000000000000000000, 0.000000000000000000, -1.000000000000000000 ) ) ;
#9266 = ORIENTED_EDGE ( 'NONE', *, *, #3390, .T. ) ;
#9267 = DIRECTION ( 'NONE',  ( 0.000000000000000000, 0.000000000000000000, 1.000000000000000000 ) ) ;
#9268 = AXIS2_PLACEMENT_3D ( 'NONE', #4559, #8589, #6201 ) ;
#9269 = DIRECTION ( 'NONE',  ( -1.000000000000000000, 0.000000000000000000, -0.000000000000000000 ) ) ;
#9270 = DIRECTION ( 'NONE',  ( 0.000000000000000000, 0.000000000000000000, -1.000000000000000000 ) ) ;
#9271 = CYLINDRICAL_SURFACE ( 'NONE', #7970, 3.999999999999989786 ) ;
#9272 = AXIS2_PLACEMENT_3D ( 'NONE', #9726, #4782, #1608 ) ;
#9273 = EDGE_LOOP ( 'NONE', ( #2839, #1607, #5372, #9137 ) ) ;
#9274 = ORIENTED_EDGE ( 'NONE', *, *, #3776, .T. ) ;
#9275 = FACE_OUTER_BOUND ( 'NONE', #207, .T. ) ;
#9276 = ORIENTED_EDGE ( 'NONE', *, *, #2883, .F. ) ;
#9277 = ADVANCED_FACE ( 'NONE', ( #9662 ), #6000, .F. ) ;
#9278 = DIRECTION ( 'NONE',  ( 0.000000000000000000, -0.000000000000000000, -1.000000000000000000 ) ) ;
#9279 =( LENGTH_UNIT ( ) NAMED_UNIT ( * ) SI_UNIT ( .MILLI., .METRE. ) );
#9280 = CIRCLE ( 'NONE', #1823, 3.999999999999989786 ) ;
#9281 = CARTESIAN_POINT ( 'NONE',  ( -23.79350689640809335, 76.32362273389503571, 54.43095569077609497 ) ) ;
#9282 = DIRECTION ( 'NONE',  ( 0.000000000000000000, -0.5000000000000012212, -0.8660254037844380415 ) ) ;
#9283 = CIRCLE ( 'NONE', #5386, 2.000000000000001776 ) ;
#9284 = EDGE_LOOP ( 'NONE', ( #661, #2183 ) ) ;
#9285 = ORIENTED_EDGE ( 'NONE', *, *, #7838, .T. ) ;
#9286 = CARTESIAN_POINT ( 'NONE',  ( -40.00000000000001421, -135.1457019118818721, -44.02500000000001990 ) ) ;
#9287 = VECTOR ( 'NONE', #4506, 1000.000000000000000 ) ;
#9288 = ORIENTED_EDGE ( 'NONE', *, *, #5006, .F. ) ;
#9289 = CIRCLE ( 'NONE', #4391, 2.515249034521771510 ) ;
#9290 = ADVANCED_FACE ( 'NONE', ( #7211 ), #5567, .T. ) ;
#9291 = DIRECTION ( 'NONE',  ( -0.000000000000000000, 1.000000000000000000, -0.000000000000000000 ) ) ;
#9292 = LINE ( 'NONE', #7800, #535 ) ;
#9293 = EDGE_CURVE ( 'NONE', #7537, #10220, #928, .T. ) ;
#9294 = EDGE_CURVE ( 'NONE', #6087, #2209, #1441, .T. ) ;
#9295 = PLANE ( 'NONE',  #1127 ) ;
#9296 = FACE_OUTER_BOUND ( 'NONE', #7694, .T. ) ;
#9297 = CARTESIAN_POINT ( 'NONE',  ( -40.00000000000001421, -135.1457019118818721, -35.97500000000002274 ) ) ;
#9298 = ORIENTED_EDGE ( 'NONE', *, *, #1516, .F. ) ;
#9299 = PRESENTATION_LAYER_ASSIGNMENT (  '', '', ( #1509 ) ) ;
#9300 = DIRECTION ( 'NONE',  ( -1.000000000000000000, -0.000000000000000000, -0.000000000000000000 ) ) ;
#9301 = CARTESIAN_POINT ( 'NONE',  ( -155.4728935706336301, 261.2517229562222951, 0.000000000000000000 ) ) ;
#9302 = PRODUCT_DEFINITION ( 'UNKNOWN', '', #1431, #7489 ) ;
#9303 = VERTEX_POINT ( 'NONE', #3227 ) ;
#9304 = EDGE_CURVE ( 'NONE', #1323, #109, #3815, .T. ) ;
#9305 = EDGE_CURVE ( 'NONE', #6600, #7930, #4866, .T. ) ;
#9306=STYLED_ITEM('',(#10497),#3077);
#9307 = APPLICATION_CONTEXT ( 'automotive_design' ) ;
#9308 = PLANE ( 'NONE',  #5188 ) ;
#9309 = DIRECTION ( 'NONE',  ( 0.000000000000000000, -0.5660304919045656691, 0.8243843049417398650 ) ) ;
#9310 = CARTESIAN_POINT ( 'NONE',  ( -8.000000000000000000, 0.000000000000000000, 0.000000000000000000 ) ) ;
#9311 = CARTESIAN_POINT ( 'NONE',  ( 14.70649310359190309, 80.56966535057935630, 20.00000000000000711 ) ) ;
#9312 = ORIENTED_EDGE ( 'NONE', *, *, #414, .T. ) ;
#9313 = CARTESIAN_POINT ( 'NONE',  ( -159.2094387399987738, 254.1279851649838122, 0.000000000000000000 ) ) ;
#9314 = EDGE_LOOP ( 'NONE', ( #5407, #9117, #5903, #6586 ) ) ;
#9315 =( NAMED_UNIT ( * ) SI_UNIT ( $, .STERADIAN. ) SOLID_ANGLE_UNIT ( ) );
#9316 = VERTEX_POINT ( 'NONE', #7060 ) ;
#9317 = CARTESIAN_POINT ( 'NONE',  ( -50.00000000000002132, -115.1457019118818863, -23.15769640663945594 ) ) ;
#9318 = ORIENTED_EDGE ( 'NONE', *, *, #9502, .T. ) ;
#9319 = EDGE_LOOP ( 'NONE', ( #3583, #3933, #1617, #9405 ) ) ;
#9320 = FACE_OUTER_BOUND ( 'NONE', #7451, .T. ) ;
#9321 = DIRECTION ( 'NONE',  ( -0.000000000000000000, -0.000000000000000000, -1.000000000000000000 ) ) ;
#9322 = LINE ( 'NONE', #6024, #7442 ) ;
#9323 = DIRECTION ( 'NONE',  ( 0.000000000000000000, 0.000000000000000000, 1.000000000000000000 ) ) ;
#9324 = CARTESIAN_POINT ( 'NONE',  ( -2.293506896408097795, 120.5696653505793705, -24.00000000000000711 ) ) ;
#9325 = CARTESIAN_POINT ( 'NONE',  ( -47.94539818030330025, 150.5446653505793790, 3.999999999999989786 ) ) ;
#9326 = ADVANCED_FACE ( 'NONE', ( #10299 ), #3027, .F. ) ;
#9327 = ORIENTED_EDGE ( 'NONE', *, *, #105, .T. ) ;
#9328 = ORIENTED_EDGE ( 'NONE', *, *, #6820, .T. ) ;
#9329 = FACE_OUTER_BOUND ( 'NONE', #6129, .T. ) ;
#9330 = VECTOR ( 'NONE', #2853, 1000.000000000000000 ) ;
#9331 = ORIENTED_EDGE ( 'NONE', *, *, #3686, .T. ) ;
#9332 = DIRECTION ( 'NONE',  ( 1.000000000000000000, 0.000000000000000000, -1.734723475976804383E-16 ) ) ;
#9333 = DIRECTION ( 'NONE',  ( 0.000000000000000000, 0.000000000000000000, 1.000000000000000000 ) ) ;
#9334 = DIRECTION ( 'NONE',  ( 0.000000000000000000, 0.000000000000000000, 1.000000000000000000 ) ) ;
#9335 = CARTESIAN_POINT ( 'NONE',  ( 37.22511195853869026, -115.1457019118818863, 23.15769640663938134 ) ) ;
#9336 = VERTEX_POINT ( 'NONE', #1691 ) ;
#9337 = ORIENTED_EDGE ( 'NONE', *, *, #356, .F. ) ;
#9338 = AXIS2_PLACEMENT_3D ( 'NONE', #10442, #7951, #9550 ) ;
#9339 = EDGE_LOOP ( 'NONE', ( #1953, #2332, #2706 ) ) ;
#9340 = AXIS2_PLACEMENT_3D ( 'NONE', #599, #7069, #3035 ) ;
#9341 = ORIENTED_EDGE ( 'NONE', *, *, #4863, .F. ) ;
#9342 = ORIENTED_EDGE ( 'NONE', *, *, #5993, .F. ) ;
#9343 = LINE ( 'NONE', #1968, #139 ) ;
#9344 = DIRECTION ( 'NONE',  ( -9.101836848464095537E-17, 0.000000000000000000, -1.000000000000000000 ) ) ;
#9345 = LINE ( 'NONE', #6796, #10439 ) ;
#9346 = DIRECTION ( 'NONE',  ( 0.7431448254773963535, -0.6691306063588559061, 0.000000000000000000 ) ) ;
#9347 = DIRECTION ( 'NONE',  ( 1.000000000000000000, -1.802741689055041147E-15, 0.000000000000000000 ) ) ;
#9348 = AXIS2_PLACEMENT_3D ( 'NONE', #5333, #6480, #3009 ) ;
#9349 = VERTEX_POINT ( 'NONE', #2595 ) ;
#9350 = DIRECTION ( 'NONE',  ( 1.000000000000000000, 0.000000000000000000, 0.000000000000000000 ) ) ;
#9351 =( BOUNDED_CURVE ( )  B_SPLINE_CURVE ( 3, ( #3319, #5061, #7346, #7295 ),
 .UNSPECIFIED., .F., .T. ) 
 B_SPLINE_CURVE_WITH_KNOTS ( ( 4, 4 ),
 ( 1.848378549510505620, 3.054692141489262713 ),
 .UNSPECIFIED. ) 
 CURVE ( )  GEOMETRIC_REPRESENTATION_ITEM ( )  RATIONAL_B_SPLINE_CURVE ( ( 1.000000000000000000, 0.8823660295963220435, 0.8823660295963220435, 1.000000000000000000 ) ) 
 REPRESENTATION_ITEM ( '' )  );
#9352 = ADVANCED_FACE ( 'NONE', ( #6513 ), #5819, .F. ) ;
#9353 = FACE_OUTER_BOUND ( 'NONE', #3646, .T. ) ;
#9354 = ORIENTED_EDGE ( 'NONE', *, *, #7267, .F. ) ;
#9355 = AXIS2_PLACEMENT_3D ( 'NONE', #658, #904, #850 ) ;
#9356 = AXIS2_PLACEMENT_3D ( 'NONE', #3323, #8993, #4226 ) ;
#9357 = CARTESIAN_POINT ( 'NONE',  ( -40.00000000000002842, -135.1457019118818721, 35.97499999999998010 ) ) ;
#9358 = DIRECTION ( 'NONE',  ( -0.000000000000000000, -1.000000000000000000, -0.000000000000000000 ) ) ;
#9359 = CARTESIAN_POINT ( 'NONE',  ( -2.293506896408097795, 120.5696653505793705, -24.00000000000000711 ) ) ;
#9360 = ORIENTED_EDGE ( 'NONE', *, *, #1696, .T. ) ;
#9361 = CARTESIAN_POINT ( 'NONE',  ( 37.22759939293836595, -117.1457019118819005, 25.15769640663938134 ) ) ;
#9362 = EDGE_CURVE ( 'NONE', #3355, #8552, #8367, .T. ) ;
#9363 = EDGE_CURVE ( 'NONE', #7873, #1605, #4968, .T. ) ;
#9364 = AXIS2_PLACEMENT_3D ( 'NONE', #7586, #4509, #8429 ) ;
#9365 = EDGE_CURVE ( 'NONE', #9778, #4565, #595, .T. ) ;
#9366 = VERTEX_POINT ( 'NONE', #2647 ) ;
#9367 = EDGE_LOOP ( 'NONE', ( #5712, #1151, #9879, #585 ) ) ;
#9368 = FACE_OUTER_BOUND ( 'NONE', #8333, .T. ) ;
#9369 = ORIENTED_EDGE ( 'NONE', *, *, #3266, .F. ) ;
#9370 = ORIENTED_EDGE ( 'NONE', *, *, #894, .F. ) ;
#9371 = DIRECTION ( 'NONE',  ( -1.000000000000000000, -0.000000000000000000, 0.000000000000000000 ) ) ;
#9372 = DIRECTION ( 'NONE',  ( -0.000000000000000000, -0.000000000000000000, -1.000000000000000000 ) ) ;
#9373 = VECTOR ( 'NONE', #7416, 1000.000000000000000 ) ;
#9374 = ORIENTED_EDGE ( 'NONE', *, *, #10315, .T. ) ;
#9375 = DIRECTION ( 'NONE',  ( 8.659560562356134638E-17, 0.7071067811864494290, -0.7071067811866454944 ) ) ;
#9376 = DIRECTION ( 'NONE',  ( 0.000000000000000000, 0.000000000000000000, -1.000000000000000000 ) ) ;
#9377 = LINE ( 'NONE', #3707, #263 ) ;
#9378 = DIRECTION ( 'NONE',  ( -0.000000000000000000, 1.000000000000000000, -0.000000000000000000 ) ) ;
#9379 = EDGE_CURVE ( 'NONE', #6373, #6699, #8030, .T. ) ;
#9380 = VERTEX_POINT ( 'NONE', #8311 ) ;
#9381 = AXIS2_PLACEMENT_3D ( 'NONE', #10430, #2367, #4651 ) ;
#9382 = DIRECTION ( 'NONE',  ( -0.7431448254773957984, 0.6691306063588565722, -0.000000000000000000 ) ) ;
#9383 = CARTESIAN_POINT ( 'NONE',  ( 14.70649310359190309, 120.5696653505793705, 20.00000000000000711 ) ) ;
#9384 = VERTEX_POINT ( 'NONE', #3389 ) ;
#9385 = CARTESIAN_POINT ( 'NONE',  ( 23.15769640663938134, -117.1457019118819005, -27.15769640663941686 ) ) ;
#9386 = CARTESIAN_POINT ( 'NONE',  ( 37.22511195853869026, -115.1457019118818863, -23.15769640663939910 ) ) ;
#9387 = DIRECTION ( 'NONE',  ( -0.000000000000000000, -1.000000000000000000, -0.000000000000000000 ) ) ;
#9388 = AXIS2_PLACEMENT_3D ( 'NONE', #4103, #7335, #1715 ) ;
#9389 = CYLINDRICAL_SURFACE ( 'NONE', #2963, 5.000000000000007994 ) ;
#9390 = ORIENTED_EDGE ( 'NONE', *, *, #6234, .F. ) ;
#9391 = EDGE_LOOP ( 'NONE', ( #9645, #1249, #7255, #8624, #9298, #4854, #450, #5642, #4031, #4114, #383, #1442, #8935, #5344, #1339, #6058 ) ) ;
#9392 = AXIS2_PLACEMENT_3D ( 'NONE', #5761, #1002, #896 ) ;
#9393 = ORIENTED_EDGE ( 'NONE', *, *, #4215, .T. ) ;
#9394 = ORIENTED_EDGE ( 'NONE', *, *, #4372, .F. ) ;
#9395 = DIRECTION ( 'NONE',  ( -1.000000000000000000, -0.000000000000000000, -0.000000000000000000 ) ) ;
#9396 = EDGE_CURVE ( 'NONE', #4437, #5933, #7869, .T. ) ;
#9397 = CARTESIAN_POINT ( 'NONE',  ( -27.85255513972543895, 90.52895752738122326, -7.749999999999996447 ) ) ;
#9398 = VECTOR ( 'NONE', #4234, 1000.000000000000000 ) ;
#9399 = CARTESIAN_POINT ( 'NONE',  ( 38.19229777560031636, 118.3760186273086816, 12.50000000000000000 ) ) ;
#9400 = CARTESIAN_POINT ( 'NONE',  ( -30.29350689640809335, 112.5696653505793705, -20.00000000000000711 ) ) ;
#9401 = ORIENTED_EDGE ( 'NONE', *, *, #5082, .T. ) ;
#9402 = LINE ( 'NONE', #3841, #3235 ) ;
#9403 = CYLINDRICAL_SURFACE ( 'NONE', #6921, 2.000000000000001776 ) ;
#9404 = EDGE_LOOP ( 'NONE', ( #8909, #10083, #5538 ) ) ;
#9405 = ORIENTED_EDGE ( 'NONE', *, *, #8527, .F. ) ;
#9406 = PRODUCT ( 'Reciprocating Punch Ram Shaft', 'Reciprocating Punch Ram Shaft', '', ( #4586 ) ) ;
#9407 = ADVANCED_FACE ( 'NONE', ( #3493 ), #9112, .F. ) ;
#9408 = AXIS2_PLACEMENT_3D ( 'NONE', #1144, #7506, #2835 ) ;
#9409 = DIRECTION ( 'NONE',  ( 0.7071067811864983899, 0.000000000000000000, 0.7071067811865966446 ) ) ;
#9410 = CARTESIAN_POINT ( 'NONE',  ( -24.31850689640809549, 140.5696653505793563, -10.90000000000000036 ) ) ;
#9411 = CARTESIAN_POINT ( 'NONE',  ( 37.22759939293836595, -117.1457019118819005, 25.15769640663938134 ) ) ;
#9412 = ORIENTED_EDGE ( 'NONE', *, *, #332, .F. ) ;
#9413 = DIRECTION ( 'NONE',  ( 0.000000000000000000, 0.000000000000000000, -1.000000000000000000 ) ) ;
#9414 = AXIS2_PLACEMENT_3D ( 'NONE', #9264, #8519, #4281 ) ;
#9415 = EDGE_LOOP ( 'NONE', ( #2545, #3405, #1545, #1390 ) ) ;
#9416 = DIRECTION ( 'NONE',  ( 1.110223024625156540E-16, -0.2829836251474256992, 0.9591247405308765961 ) ) ;
#9417 = ORIENTED_EDGE ( 'NONE', *, *, #5270, .F. ) ;
#9418 = AXIS2_PLACEMENT_3D ( 'NONE', #7702, #1924, #5155 ) ;
#9419 = CARTESIAN_POINT ( 'NONE',  ( -7.293506896408097795, 2.445795361565304815E-15, -20.00000000000002132 ) ) ;
#9420 = EDGE_LOOP ( 'NONE', ( #7488, #6204, #6303, #9571 ) ) ;
#9421 = ORIENTED_EDGE ( 'NONE', *, *, #2583, .T. ) ;
#9422 = CARTESIAN_POINT ( 'NONE',  ( -36.36957570605426326, 137.0132282531173473, 0.000000000000000000 ) ) ;
#9423 = EDGE_CURVE ( 'NONE', #3840, #8901, #8715, .T. ) ;
#9424 = CYLINDRICAL_SURFACE ( 'NONE', #4446, 4.729641367753004033 ) ;
#9425 = ADVANCED_FACE ( 'NONE', ( #6724 ), #1798, .F. ) ;
#9426 = EDGE_LOOP ( 'NONE', ( #7009, #571, #5171, #3955 ) ) ;
#9427 = ADVANCED_FACE ( 'NONE', ( #4132, #4911 ), #4185, .T. ) ;
#9428 = CARTESIAN_POINT ( 'NONE',  ( -23.76520584195948516, -145.1457019118819005, -97.78965767959371647 ) ) ;
#9429 = FACE_OUTER_BOUND ( 'NONE', #10316, .T. ) ;
#9430 = CARTESIAN_POINT ( 'NONE',  ( -48.00000000000002132, -133.1457019118818721, -23.15769640663945594 ) ) ;
#9431 = CIRCLE ( 'NONE', #6033, 4.999999999999995559 ) ;
#9432 = CARTESIAN_POINT ( 'NONE',  ( -16.29350689640809691, 76.32362273389503571, 0.000000000000000000 ) ) ;
#9433 = CARTESIAN_POINT ( 'NONE',  ( -144.3846363017538010, 149.5413575692592474, 0.000000000000000000 ) ) ;
#9434 = ORIENTED_EDGE ( 'NONE', *, *, #964, .T. ) ;
#9435 = CIRCLE ( 'NONE', #2656, 3.999999999999989786 ) ;
#9436 = DIRECTION ( 'NONE',  ( -1.000000000000000000, -0.000000000000000000, -0.000000000000000000 ) ) ;
#9437 = VERTEX_POINT ( 'NONE', #1050 ) ;
#9438 = EDGE_CURVE ( 'NONE', #8738, #2339, #3644, .T. ) ;
#9439 = FACE_OUTER_BOUND ( 'NONE', #3272, .T. ) ;
#9440 = FACE_OUTER_BOUND ( 'NONE', #8346, .T. ) ;
#9441 =( LENGTH_UNIT ( ) NAMED_UNIT ( * ) SI_UNIT ( .MILLI., .METRE. ) );
#9442 = EDGE_CURVE ( 'NONE', #2474, #8605, #57, .T. ) ;
#9443 = CARTESIAN_POINT ( 'NONE',  ( -50.00000000000002842, -134.6884760388430777, 24.98775663295401372 ) ) ;
#9444 = CARTESIAN_POINT ( 'NONE',  ( -2.293506896408097795, 80.56966535057935630, -16.00000000000000711 ) ) ;
#9445 = VECTOR ( 'NONE', #8712, 999.9999999999998863 ) ;
#9446 = DIRECTION ( 'NONE',  ( -0.000000000000000000, -1.000000000000000000, -0.000000000000000000 ) ) ;
#9447 = ORIENTED_EDGE ( 'NONE', *, *, #287, .T. ) ;
#9448 = VERTEX_POINT ( 'NONE', #4075 ) ;
#9449 = CIRCLE ( 'NONE', #4697, 7.728925574020643730 ) ;
#9450 = VECTOR ( 'NONE', #6466, 1000.000000000000000 ) ;
#9451 = EDGE_LOOP ( 'NONE', ( #10294, #4490, #1813, #5663 ) ) ;
#9452 = VERTEX_POINT ( 'NONE', #215 ) ;
#9453 = DIRECTION ( 'NONE',  ( 0.000000000000000000, 0.000000000000000000, 1.000000000000000000 ) ) ;
#9454 = CARTESIAN_POINT ( 'NONE',  ( 23.39899473324886614, -133.3869996355172987, 49.99999999999998579 ) ) ;
#9455 = DIRECTION ( 'NONE',  ( -1.000000000000000000, -0.000000000000000000, 0.000000000000000000 ) ) ;
#9456 = CARTESIAN_POINT ( 'NONE',  ( -67.94539818030330025, 155.5289575273812090, 0.000000000000000000 ) ) ;
#9457 = CARTESIAN_POINT ( 'NONE',  ( 23.15769640663940265, -133.1457019118818721, -50.00000000000002132 ) ) ;
#9458 = VECTOR ( 'NONE', #6143, 1000.000000000000000 ) ;
#9459 = VERTEX_POINT ( 'NONE', #2537 ) ;
#9460 = CARTESIAN_POINT ( 'NONE',  ( 77.30044127146540234, 73.68369600860394542, -24.99999999999998934 ) ) ;
#9461 = EDGE_CURVE ( 'NONE', #5603, #4450, #5932, .T. ) ;
#9462 = VERTEX_POINT ( 'NONE', #1744 ) ;
#9463 = LINE ( 'NONE', #8500, #5026 ) ;
#9464 = DIRECTION ( 'NONE',  ( 0.6585271261848804070, -0.7525569905852198538, 0.000000000000000000 ) ) ;
#9465 = AXIS2_PLACEMENT_3D ( 'NONE', #8131, #980, #5850 ) ;
#9466 = CARTESIAN_POINT ( 'NONE',  ( 23.64292728780886321, -133.6309146189979060, -50.00000000000002842 ) ) ;
#9467 = CARTESIAN_POINT ( 'NONE',  ( -16.29350689640809691, 11.33971203780352255, 0.000000000000000000 ) ) ;
#9468 = ORIENTED_EDGE ( 'NONE', *, *, #373, .F. ) ;
#9469 = LINE ( 'NONE', #7977, #9873 ) ;
#9470 = ORIENTED_EDGE ( 'NONE', *, *, #2200, .F. ) ;
#9471 = APPLICATION_PROTOCOL_DEFINITION ( 'draft international standard', 'automotive_design', 1998, #9516 ) ;
#9472 = EDGE_CURVE ( 'NONE', #5429, #5925, #270, .T. ) ;
#9473 = ORIENTED_EDGE ( 'NONE', *, *, #2944, .F. ) ;
#9474 = CARTESIAN_POINT ( 'NONE',  ( -16.29350689640810756, 140.5696653505793563, -20.00000000000000711 ) ) ;
#9475 = AXIS2_PLACEMENT_3D ( 'NONE', #5888, #5094, #1070 ) ;
#9476 = ORIENTED_EDGE ( 'NONE', *, *, #3024, .T. ) ;
#9477 = VERTEX_POINT ( 'NONE', #5870 ) ;
#9478 = CARTESIAN_POINT ( 'NONE',  ( -16.29350689640809691, -186.9457019118818835, -30.31717237747080773 ) ) ;
#9479 = CARTESIAN_POINT ( 'NONE',  ( 37.22759939293836595, -135.1457019118818721, 25.15769640663938134 ) ) ;
#9480 = VERTEX_POINT ( 'NONE', #3551 ) ;
#9481 = CARTESIAN_POINT ( 'NONE',  ( -47.94539818030330025, 150.5696653505793563, -4.025000000000000355 ) ) ;
#9482 = CARTESIAN_POINT ( 'NONE',  ( -136.0474385147828116, 266.3109523634597622, 0.000000000000000000 ) ) ;
#9483 = ADVANCED_FACE ( 'NONE', ( #5975 ), #6993, .T. ) ;
#9484 = CARTESIAN_POINT ( 'NONE',  ( -23.15769640663940976, -133.1457019118818721, 47.99999999999997868 ) ) ;
#9485 = CARTESIAN_POINT ( 'NONE',  ( 37.22511195853869026, -145.1457019118819005, 30.00000000000000355 ) ) ;
#9486 = DIRECTION ( 'NONE',  ( 0.000000000000000000, 0.000000000000000000, 1.000000000000000000 ) ) ;
#9487 = EDGE_CURVE ( 'NONE', #9303, #10082, #10354, .T. ) ;
#9488 = VERTEX_POINT ( 'NONE', #7576 ) ;
#9489 = EDGE_CURVE ( 'NONE', #8144, #4377, #423, .T. ) ;
#9490 = CARTESIAN_POINT ( 'NONE',  ( -25.15769640663937423, -135.1457019118818721, -48.00000000000002132 ) ) ;
#9491 = VERTEX_POINT ( 'NONE', #4398 ) ;
#9492 = DIRECTION ( 'NONE',  ( 0.07334937666141724821, -0.9973063064792989652, -0.000000000000000000 ) ) ;
#9493 = DIRECTION ( 'NONE',  ( -1.000000000000000000, 0.000000000000000000, 0.000000000000000000 ) ) ;
#9494 =( NAMED_UNIT ( * ) PLANE_ANGLE_UNIT ( ) SI_UNIT ( $, .RADIAN. ) );
#9495 = VERTEX_POINT ( 'NONE', #326 ) ;
#9496 = DIRECTION ( 'NONE',  ( 0.000000000000000000, -1.329743448921561232E-15, -1.000000000000000000 ) ) ;
#9497 = CARTESIAN_POINT ( 'NONE',  ( 38.19229777560031636, -43.28483205141633761, 12.50000000000000000 ) ) ;
#9498 = DIRECTION ( 'NONE',  ( 0.000000000000000000, 1.000000000000000000, 0.000000000000000000 ) ) ;
#9499 = EDGE_LOOP ( 'NONE', ( #1202, #6533, #2349, #2969 ) ) ;
#9500 = ORIENTED_EDGE ( 'NONE', *, *, #7208, .T. ) ;
#9501 = EDGE_CURVE ( 'NONE', #5649, #10246, #8576, .T. ) ;
#9502 = EDGE_CURVE ( 'NONE', #493, #2212, #365, .T. ) ;
#9503 = EDGE_CURVE ( 'NONE', #9495, #7867, #2843, .T. ) ;
#9504 = PRODUCT_DEFINITION_SHAPE ( 'NONE', 'NONE',  #6322 ) ;
#9505 = ORIENTED_EDGE ( 'NONE', *, *, #8261, .F. ) ;
#9506 = VERTEX_POINT ( 'NONE', #8420 ) ;
#9507 = FACE_OUTER_BOUND ( 'NONE', #3495, .T. ) ;
#9508 = CARTESIAN_POINT ( 'NONE',  ( -38.96131932220313132, -0.2735269159956721374, 3.990636919869543942 ) ) ;
#9509 = VECTOR ( 'NONE', #201, 1000.000000000000000 ) ;
#9510 = DIRECTION ( 'NONE',  ( 0.7525569905852205199, 0.6585271261848794078, 0.000000000000000000 ) ) ;
#9511 = DIRECTION ( 'NONE',  ( -1.000000000000000000, 0.000000000000000000, 0.000000000000000000 ) ) ;
#9512 = DIRECTION ( 'NONE',  ( 0.000000000000000000, 0.000000000000000000, -1.000000000000000000 ) ) ;
#9513 = VERTEX_POINT ( 'NONE', #9325 ) ;
#9514 = DIRECTION ( 'NONE',  ( 1.000000000000000000, 0.000000000000000000, 0.000000000000000000 ) ) ;
#9515 = AXIS2_PLACEMENT_3D ( 'NONE', #7761, #6801, #9245 ) ;
#9516 = APPLICATION_CONTEXT ( 'automotive_design' ) ;
#9517 = EDGE_CURVE ( 'NONE', #6524, #6151, #2041, .T. ) ;
#9518 = AXIS2_PLACEMENT_3D ( 'NONE', #969, #4306, #7541 ) ;
#9519 = ORIENTED_EDGE ( 'NONE', *, *, #691, .T. ) ;
#9520 = FACE_OUTER_BOUND ( 'NONE', #7503, .T. ) ;
#9521 = EDGE_CURVE ( 'NONE', #5490, #3561, #1204, .T. ) ;
#9522 = LINE ( 'NONE', #7766, #1485 ) ;
#9523 = AXIS2_PLACEMENT_3D ( 'NONE', #7962, #6318, #8701 ) ;
#9524 = CARTESIAN_POINT ( 'NONE',  ( -23.79350689640810046, 76.32362273389503571, 7.750000000000007105 ) ) ;
#9525 = DIRECTION ( 'NONE',  ( -1.000000000000000000, -0.000000000000000000, -0.000000000000000000 ) ) ;
#9526 = ORIENTED_EDGE ( 'NONE', *, *, #10155, .F. ) ;
#9527 = CYLINDRICAL_SURFACE ( 'NONE', #8160, 2.000000000000001776 ) ;
#9528 = DIRECTION ( 'NONE',  ( -4.105177310309856893E-17, -0.5365380858086067350, 0.8438761061179753664 ) ) ;
#9529 = VERTEX_POINT ( 'NONE', #10174 ) ;
#9530 = VECTOR ( 'NONE', #10119, 1000.000000000000000 ) ;
#9531 = CARTESIAN_POINT ( 'NONE',  ( -27.15769640663940976, -117.1457019118819005, 25.15769640663938134 ) ) ;
#9532 = CIRCLE ( 'NONE', #10200, 10.00000000000000888 ) ;
#9533 = ORIENTED_EDGE ( 'NONE', *, *, #3837, .T. ) ;
#9534 = VERTEX_POINT ( 'NONE', #6830 ) ;
#9535 = CARTESIAN_POINT ( 'NONE',  ( 25.15769640663938134, -117.1457019118819005, -27.15769640663941331 ) ) ;
#9536 = CARTESIAN_POINT ( 'NONE',  ( 25.15769640663936713, -115.1457019118818863, 47.99999999999997868 ) ) ;
#9537 = EDGE_CURVE ( 'NONE', #5925, #6085, #1706, .T. ) ;
#9538 = DIRECTION ( 'NONE',  ( -1.000000000000000000, 0.000000000000000000, 0.000000000000000000 ) ) ;
#9539 = DIRECTION ( 'NONE',  ( 0.000000000000000000, -0.000000000000000000, -1.000000000000000000 ) ) ;
#9540 = DIRECTION ( 'NONE',  ( 0.000000000000000000, -1.000000000000000000, -9.100899318238110877E-17 ) ) ;
#9541 = AXIS2_PLACEMENT_3D ( 'NONE', #2346, #702, #3088 ) ;
#9542 = DIRECTION ( 'NONE',  ( -1.000000000000000000, -1.734723475976801918E-16, 1.734723475976813997E-16 ) ) ;
#9543 = VECTOR ( 'NONE', #10041, 1000.000000000000000 ) ;
#9544 = CARTESIAN_POINT ( 'NONE',  ( -30.29350689640809335, 80.56966535057935630, -20.00000000000000711 ) ) ;
#9545 = ORIENTED_EDGE ( 'NONE', *, *, #5859, .F. ) ;
#9546 = DIRECTION ( 'NONE',  ( -0.000000000000000000, -0.000000000000000000, -1.000000000000000000 ) ) ;
#9547 = VECTOR ( 'NONE', #1276, 1000.000000000000000 ) ;
#9548 = ORIENTED_EDGE ( 'NONE', *, *, #5629, .F. ) ;
#9549 = DIRECTION ( 'NONE',  ( 1.137729606058012035E-16, 0.000000000000000000, 1.000000000000000000 ) ) ;
#9550 = DIRECTION ( 'NONE',  ( 0.000000000000000000, 0.000000000000000000, -1.000000000000000000 ) ) ;
#9551 =( NAMED_UNIT ( * ) PLANE_ANGLE_UNIT ( ) SI_UNIT ( $, .RADIAN. ) );
#9552 = CARTESIAN_POINT ( 'NONE',  ( -18.34874108452141783, -140.1746510883711778, -97.78965767959371647 ) ) ;
#9553 = EDGE_CURVE ( 'NONE', #1218, #6270, #1211, .T. ) ;
#9554 = CARTESIAN_POINT ( 'NONE',  ( 14.70649310359190309, 120.5696653505793705, -20.00000000000000711 ) ) ;
#9555 = DIRECTION ( 'NONE',  ( -6.982941293900105430E-16, 0.000000000000000000, 1.000000000000000000 ) ) ;
#9556 = VERTEX_POINT ( 'NONE', #2054 ) ;
#9557 = VECTOR ( 'NONE', #3437, 1000.000000000000000 ) ;
#9558 = ORIENTED_EDGE ( 'NONE', *, *, #9885, .F. ) ;
#9559 =( GEOMETRIC_REPRESENTATION_CONTEXT ( 3 ) GLOBAL_UNCERTAINTY_ASSIGNED_CONTEXT ( ( #9073 ) ) GLOBAL_UNIT_ASSIGNED_CONTEXT ( ( #3530, #2724, #6706 ) ) REPRESENTATION_CONTEXT ( 'NONE', 'WORKASPACE' ) );
#9560 = ORIENTED_EDGE ( 'NONE', *, *, #8300, .T. ) ;
#9561 = ORIENTED_EDGE ( 'NONE', *, *, #7327, .F. ) ;
#9562 = CARTESIAN_POINT ( 'NONE',  ( 37.22511195853866894, 17.84145331825995484, 30.00000000000000355 ) ) ;
#9563 = CARTESIAN_POINT ( 'NONE',  ( -1.071796769724492338, -0.2735269159956698060, 3.990636919869545718 ) ) ;
#9564 = AXIS2_PLACEMENT_3D ( 'NONE', #9799, #5854, #9093 ) ;
#9565 = DIRECTION ( 'NONE',  ( -0.6691306063588553510, -0.7431448254773969087, 0.000000000000000000 ) ) ;
#9566 = CARTESIAN_POINT ( 'NONE',  ( -56.36957570605427037, 137.0132282531173473, 0.000000000000000000 ) ) ;
#9567 = ADVANCED_FACE ( 'NONE', ( #6028 ), #9271, .F. ) ;
#9568 = EDGE_CURVE ( 'NONE', #1563, #6846, #4448, .T. ) ;
#9569 = ADVANCED_FACE ( 'NONE', ( #7732, #474, #2112 ), #3709, .T. ) ;
#9570 = DIRECTION ( 'NONE',  ( 0.000000000000000000, 0.000000000000000000, 1.000000000000000000 ) ) ;
#9571 = ORIENTED_EDGE ( 'NONE', *, *, #8448, .F. ) ;
#9572 = CYLINDRICAL_SURFACE ( 'NONE', #10360, 19.24539146688411506 ) ;
#9573 = CIRCLE ( 'NONE', #250, 5.000000000000004441 ) ;
#9574 = ORIENTED_EDGE ( 'NONE', *, *, #3459, .T. ) ;
#9575 = EDGE_CURVE ( 'NONE', #5184, #7686, #7783, .T. ) ;
#9576 = DIRECTION ( 'NONE',  ( -1.000000000000000000, 0.000000000000000000, 0.000000000000000000 ) ) ;
#9577 = VECTOR ( 'NONE', #7117, 1000.000000000000000 ) ;
#9578 = EDGE_CURVE ( 'NONE', #9915, #2553, #6101, .T. ) ;
#9579 = CARTESIAN_POINT ( 'NONE',  ( 17.97972049165455388, 42.08684478514406635, 25.00000000000000000 ) ) ;
#9580 = CARTESIAN_POINT ( 'NONE',  ( 37.22511195853866894, 17.84145331825995839, 30.00000000000000355 ) ) ;
#9581 = FACE_OUTER_BOUND ( 'NONE', #4499, .T. ) ;
#9582 = VERTEX_POINT ( 'NONE', #1533 ) ;
#9583 = DIRECTION ( 'NONE',  ( 1.000000000000000000, -0.000000000000000000, 0.000000000000000000 ) ) ;
#9584 = APPLICATION_PROTOCOL_DEFINITION ( 'draft international standard', 'automotive_design', 1998, #646 ) ;
#9585 = EDGE_LOOP ( 'NONE', ( #1629, #9012, #3473, #3392 ) ) ;
#9586 = DIRECTION ( 'NONE',  ( -0.000000000000000000, 1.000000000000000000, -0.000000000000000000 ) ) ;
#9587 = EDGE_LOOP ( 'NONE', ( #6500, #5290, #6769, #2977 ) ) ;
#9588 = AXIS2_PLACEMENT_3D ( 'NONE', #7135, #6277, #3850 ) ;
#9589 = ORIENTED_EDGE ( 'NONE', *, *, #5041, .T. ) ;
#9590 = LINE ( 'NONE', #4702, #5679 ) ;
#9591 = FACE_OUTER_BOUND ( 'NONE', #1268, .T. ) ;
#9592 = CARTESIAN_POINT ( 'NONE',  ( 14.70649310359190309, 80.56966535057935630, 20.00000000000000711 ) ) ;
#9593 = DIRECTION ( 'NONE',  ( 1.000000000000000000, -0.000000000000000000, -0.000000000000000000 ) ) ;
#9594 = VECTOR ( 'NONE', #2509, 1000.000000000000000 ) ;
#9595 = DIRECTION ( 'NONE',  ( -1.000000000000000000, 0.000000000000000000, 0.000000000000000000 ) ) ;
#9596 = DIRECTION ( 'NONE',  ( -0.7431448254773957984, 0.6691306063588565722, -0.000000000000000000 ) ) ;
#9597 = PRODUCT_DEFINITION_SHAPE ( 'NONE', 'NONE',  #9302 ) ;
#9598 = VECTOR ( 'NONE', #4368, 999.9999999999998863 ) ;
#9599 = ADVANCED_FACE ( 'NONE', ( #3813 ), #3165, .T. ) ;
#9600 = EDGE_LOOP ( 'NONE', ( #2748, #6105 ) ) ;
#9601 = CARTESIAN_POINT ( 'NONE',  ( -7.293506896408097795, 72.08684478514408056, -28.00000000000001421 ) ) ;
#9602 = AXIS2_PLACEMENT_3D ( 'NONE', #6400, #8142, #3809 ) ;
#9603 = ORIENTED_EDGE ( 'NONE', *, *, #7411, .F. ) ;
#9604 = CARTESIAN_POINT ( 'NONE',  ( -20.29350689640809691, 140.5696653505793563, -10.90000000000000036 ) ) ;
#9605 = PRESENTATION_STYLE_ASSIGNMENT (( #2334 ) ) ;
#9606 = AXIS2_PLACEMENT_3D ( 'NONE', #4090, #7376, #808 ) ;
#9607 = VERTEX_POINT ( 'NONE', #3966 ) ;
#9608 = FACE_OUTER_BOUND ( 'NONE', #2799, .T. ) ;
#9609 = LINE ( 'NONE', #8849, #4659 ) ;
#9610 = CARTESIAN_POINT ( 'NONE',  ( -56.36957570605427037, 137.0132282531173473, 0.000000000000000000 ) ) ;
#9611 = ORIENTED_EDGE ( 'NONE', *, *, #2121, .T. ) ;
#9612 = AXIS2_PLACEMENT_3D ( 'NONE', #4487, #10271, #3003 ) ;
#9613 = ORIENTED_EDGE ( 'NONE', *, *, #556, .F. ) ;
#9614 = AXIS2_PLACEMENT_3D ( 'NONE', #1780, #9850, #9733 ) ;
#9615 = EDGE_CURVE ( 'NONE', #1282, #6490, #8833, .T. ) ;
#9616 = VERTEX_POINT ( 'NONE', #2216 ) ;
#9617 = DIRECTION ( 'NONE',  ( 0.000000000000000000, -0.000000000000000000, -1.000000000000000000 ) ) ;
#9618 = DIRECTION ( 'NONE',  ( -0.07334937666141724821, 0.9973063064792989652, 0.000000000000000000 ) ) ;
#9619 = CLOSED_SHELL ( 'NONE', ( #3870, #9326, #4534, #4757, #3852, #6967, #4564, #8750, #2737, #5421, #6159, #8462, #3414, #9722, #6819, #3596, #545, #489, #9128, #4502, #3523, #1845, #1654, #2235, #5084, #2292, #1468, #6189, #9963, #7633, #3474, #4164, #5949, #10073, #5057, #89, #9737, #5683, #9903, #6855, #2109, #4428, #4876, #10203, #4488, #676, #1773, #7095, #5820, #3527, #1407, #2535 ) ) ;
#9620 = CARTESIAN_POINT ( 'NONE',  ( -25.93998375192765948, -135.0799149511624364, -50.00000000000002842 ) ) ;
#9621 = DIRECTION ( 'NONE',  ( 1.000000000000000000, 0.000000000000000000, 0.000000000000000000 ) ) ;
#9622 = CIRCLE ( 'NONE', #3345, 3.999999999999996447 ) ;
#9623 = CARTESIAN_POINT ( 'NONE',  ( 0.3000000000000016542, 0.000000000000000000, 0.000000000000000000 ) ) ;
#9624 = ORIENTED_EDGE ( 'NONE', *, *, #9489, .T. ) ;
#9625 = CARTESIAN_POINT ( 'NONE',  ( 3.000000000000000000, -2.935248768560057009, 4.770489558936219510E-15 ) ) ;
#9626 = AXIS2_PLACEMENT_3D ( 'NONE', #1391, #5573, #8007 ) ;
#9627 = ADVANCED_FACE ( 'NONE', ( #7200 ), #4749, .T. ) ;
#9628 = ADVANCED_FACE ( 'NONE', ( #578, #8035, #6348 ), #8734, .F. ) ;
#9629 = EDGE_LOOP ( 'NONE', ( #1196, #1418, #8900, #4505 ) ) ;
#9630 = PLANE ( 'NONE',  #6725 ) ;
#9631 = AXIS2_PLACEMENT_3D ( 'NONE', #6780, #378, #9332 ) ;
#9632 = CARTESIAN_POINT ( 'NONE',  ( 39.99999999999997158, -135.1707019118818778, 39.99999999999997868 ) ) ;
#9633 = CARTESIAN_POINT ( 'NONE',  ( -136.1699968855118357, 255.5531976154833274, 1.063156219295426707E-15 ) ) ;
#9634 = EDGE_LOOP ( 'NONE', ( #3714, #550, #3640, #4805 ) ) ;
#9635 = DIRECTION ( 'NONE',  ( 0.000000000000000000, 1.000000000000000000, 0.000000000000000000 ) ) ;
#9636 = DIRECTION ( 'NONE',  ( 0.000000000000000000, 0.000000000000000000, 1.000000000000000000 ) ) ;
#9637 = EDGE_CURVE ( 'NONE', #5715, #6490, #6396, .T. ) ;
#9639 = EDGE_CURVE ( 'NONE', #2017, #2815, #9674, .T. ) ;
#9638 = EDGE_LOOP ( 'NONE', ( #2257, #5071, #875, #7697 ) ) ;
#9640 = VECTOR ( 'NONE', #8948, 1000.000000000000000 ) ;
#9641 = ADVANCED_FACE ( 'NONE', ( #3215 ), #7987, .F. ) ;
#9642 = DIRECTION ( 'NONE',  ( -0.000000000000000000, -0.000000000000000000, 1.000000000000000000 ) ) ;
#9643 = ORIENTED_EDGE ( 'NONE', *, *, #1177, .T. ) ;
#9644 = CIRCLE ( 'NONE', #5052, 7.572730065532343069 ) ;
#9645 = ORIENTED_EDGE ( 'NONE', *, *, #3673, .T. ) ;
#9646 = DIRECTION ( 'NONE',  ( -1.000000000000000000, -0.000000000000000000, -0.000000000000000000 ) ) ;
#9647 = DIRECTION ( 'NONE',  ( 1.000000000000000000, 0.000000000000000000, 0.000000000000000000 ) ) ;
#9648 = CARTESIAN_POINT ( 'NONE',  ( -1.071796769724492338, 4.000000000000000000, 0.000000000000000000 ) ) ;
#9649 = DIRECTION ( 'NONE',  ( 0.000000000000000000, 0.000000000000000000, 1.000000000000000000 ) ) ;
#9650 = DIRECTION ( 'NONE',  ( 1.000000000000000000, 0.000000000000000000, 0.000000000000000000 ) ) ;
#9651 = CIRCLE ( 'NONE', #502, 5.000000000000004441 ) ;
#9652 = ORIENTED_EDGE ( 'NONE', *, *, #5411, .T. ) ;
#9653 = EDGE_CURVE ( 'NONE', #8659, #6555, #10179, .T. ) ;
#9654 = DIRECTION ( 'NONE',  ( -0.000000000000000000, 1.000000000000000000, -0.000000000000000000 ) ) ;
#9655 = VERTEX_POINT ( 'NONE', #682 ) ;
#9656 = DIRECTION ( 'NONE',  ( 0.000000000000000000, 0.000000000000000000, 1.000000000000000000 ) ) ;
#9657 = DIRECTION ( 'NONE',  ( -0.000000000000000000, -0.000000000000000000, 1.000000000000000000 ) ) ;
#9658 = AXIS2_PLACEMENT_3D ( 'NONE', #6827, #5336, #6937 ) ;
#9659 = DIRECTION ( 'NONE',  ( -0.000000000000000000, -0.000000000000000000, -1.000000000000000000 ) ) ;
#9660 = EDGE_CURVE ( 'NONE', #4536, #1149, #5430, .T. ) ;
#9661 = CARTESIAN_POINT ( 'NONE',  ( 39.99999999999998579, -135.1457019118818721, -40.00000000000002132 ) ) ;
#9662 = FACE_OUTER_BOUND ( 'NONE', #7216, .T. ) ;
#9663 = ORIENTED_EDGE ( 'NONE', *, *, #5425, .F. ) ;
#9664 = ORIENTED_EDGE ( 'NONE', *, *, #7497, .F. ) ;
#9665 = ORIENTED_EDGE ( 'NONE', *, *, #6629, .T. ) ;
#9666 = DIRECTION ( 'NONE',  ( 0.000000000000000000, -1.000000000000000000, 0.000000000000000000 ) ) ;
#9667 = CARTESIAN_POINT ( 'NONE',  ( 26.27514435518734004, -135.1457019118818437, 49.99999999999997158 ) ) ;
#9668 = CARTESIAN_POINT ( 'NONE',  ( -26.27514435518734004, -135.1457019118818437, -50.00000000000001421 ) ) ;
#9669 = DIRECTION ( 'NONE',  ( -1.000000000000000000, -0.000000000000000000, -0.000000000000000000 ) ) ;
#9670 = CARTESIAN_POINT ( 'NONE',  ( -40.00000000000001421, -135.1457019118818721, -40.00000000000002132 ) ) ;
#9671 = EDGE_LOOP ( 'NONE', ( #925, #6925, #4802, #5256 ) ) ;
#9672 = CARTESIAN_POINT ( 'NONE',  ( -47.94539818030330025, 150.5696653505793563, -3.999999999999993339 ) ) ;
#9673 = ORIENTED_EDGE ( 'NONE', *, *, #4504, .T. ) ;
#9674 = CIRCLE ( 'NONE', #7294, 7.525240063345735031 ) ;
#9675 = EDGE_LOOP ( 'NONE', ( #501, #6985, #8824, #2195, #5093, #6844 ) ) ;
#9676 = ORIENTED_EDGE ( 'NONE', *, *, #8640, .T. ) ;
#9677 = FACE_OUTER_BOUND ( 'NONE', #2202, .T. ) ;
#9678 = DIRECTION ( 'NONE',  ( -0.000000000000000000, -1.000000000000000000, -0.000000000000000000 ) ) ;
#9679 = EDGE_CURVE ( 'NONE', #5755, #5017, #7945, .T. ) ;
#9680 = FACE_OUTER_BOUND ( 'NONE', #10170, .T. ) ;
#9681 = VECTOR ( 'NONE', #4570, 1000.000000000000000 ) ;
#9682 = LINE ( 'NONE', #6649, #4084 ) ;
#9683 = ORIENTED_EDGE ( 'NONE', *, *, #4605, .F. ) ;
#9684 = DIRECTION ( 'NONE',  ( 0.000000000000000000, 0.000000000000000000, 1.000000000000000000 ) ) ;
#9685 = ORIENTED_EDGE ( 'NONE', *, *, #1395, .F. ) ;
#9686 = VECTOR ( 'NONE', #8606, 1000.000000000000000 ) ;
#9687 =( GEOMETRIC_REPRESENTATION_CONTEXT ( 3 ) GLOBAL_UNCERTAINTY_ASSIGNED_CONTEXT ( ( #5781 ) ) GLOBAL_UNIT_ASSIGNED_CONTEXT ( ( #3234, #903, #117 ) ) REPRESENTATION_CONTEXT ( 'NONE', 'WORKASPACE' ) );
#9688 = FACE_BOUND ( 'NONE', #8038, .T. ) ;
#9689 = CARTESIAN_POINT ( 'NONE',  ( -27.15769640663941331, -133.1457019118818721, 47.99999999999997868 ) ) ;
#9690 = ADVANCED_FACE ( 'NONE', ( #7890, #7835, #3016 ), #631, .F. ) ;
#9691 = EDGE_CURVE ( 'NONE', #5461, #4081, #777, .T. ) ;
#9692 = CARTESIAN_POINT ( 'NONE',  ( 49.99999999999997158, -145.1457019118819005, 39.99999999999997868 ) ) ;
#9693 = ADVANCED_FACE ( 'NONE', ( #7150 ), #10383, .T. ) ;
#9694 = DIRECTION ( 'NONE',  ( 0.000000000000000000, 0.000000000000000000, 1.000000000000000000 ) ) ;
#9695 = AXIS2_PLACEMENT_3D ( 'NONE', #136, #5047, #7544 ) ;
#9696 = AXIS2_PLACEMENT_3D ( 'NONE', #1250, #6173, #1939 ) ;
#9697 = SHAPE_REPRESENTATION ( 'Plastic Grip', ( #4601 ), #9559 ) ;
#9698 = ORIENTED_EDGE ( 'NONE', *, *, #1199, .F. ) ;
#9699 = CARTESIAN_POINT ( 'NONE',  ( -56.36957570605427037, 137.0132282531173473, 3.999999999999989786 ) ) ;
#9700 = ORIENTED_EDGE ( 'NONE', *, *, #3109, .F. ) ;
#9701 = CARTESIAN_POINT ( 'NONE',  ( -16.29350689640809691, 11.33971203780352255, -4.999999999999993783 ) ) ;
#9702 = FACE_OUTER_BOUND ( 'NONE', #3196, .T. ) ;
#9703 = AXIS2_PLACEMENT_3D ( 'NONE', #6158, #4522, #1184 ) ;
#9704 = SURFACE_STYLE_FILL_AREA ( #8895 ) ;
#9705 = CIRCLE ( 'NONE', #26, 20.00000000000000000 ) ;
#9706 = DIRECTION ( 'NONE',  ( -0.000000000000000000, -0.000000000000000000, -1.000000000000000000 ) ) ;
#9707 = DIRECTION ( 'NONE',  ( 1.000000000000000000, 0.000000000000000000, 0.000000000000000000 ) ) ;
#9708 = EDGE_CURVE ( 'NONE', #716, #5577, #4018, .T. ) ;
#9709 = ORIENTED_EDGE ( 'NONE', *, *, #6760, .F. ) ;
#9710 = ORIENTED_EDGE ( 'NONE', *, *, #4668, .F. ) ;
#9711 = ORIENTED_EDGE ( 'NONE', *, *, #7068, .T. ) ;
#9712 = CIRCLE ( 'NONE', #5128, 3.999999999999999112 ) ;
#9713 = EDGE_LOOP ( 'NONE', ( #9574, #3506, #2704, #1432 ) ) ;
#9714 = CARTESIAN_POINT ( 'NONE',  ( -50.00000000000002132, -145.1457019118819005, -6.938893903907231533E-15 ) ) ;
#9715 = DIRECTION ( 'NONE',  ( 0.000000000000000000, 0.000000000000000000, -1.000000000000000000 ) ) ;
#9716 = CARTESIAN_POINT ( 'NONE',  ( -67.94539818030330025, 155.5289575273812090, -4.898587196589412829E-16 ) ) ;
#9717 = AXIS2_PLACEMENT_3D ( 'NONE', #2902, #4547, #7781 ) ;
#9718 = ORIENTED_EDGE ( 'NONE', *, *, #8121, .F. ) ;
#9719 = DIRECTION ( 'NONE',  ( 0.000000000000000000, -0.4999999999999985567, 0.8660254037844394848 ) ) ;
#9720 = ORIENTED_EDGE ( 'NONE', *, *, #9708, .T. ) ;
#9721 = DIRECTION ( 'NONE',  ( -1.000000000000000000, 0.000000000000000000, 0.000000000000000000 ) ) ;
#9722 = ADVANCED_FACE ( 'NONE', ( #5063 ), #9098, .T. ) ;
#9723 = CIRCLE ( 'NONE', #2276, 5.000000000000002665 ) ;
#9724 = ORIENTED_EDGE ( 'NONE', *, *, #833, .F. ) ;
#9725 = ORIENTED_EDGE ( 'NONE', *, *, #373, .T. ) ;
#9726 = CARTESIAN_POINT ( 'NONE',  ( -48.00000000000002132, -133.1457019118818721, 23.15769640663938134 ) ) ;
#9727 = AXIS2_PLACEMENT_3D ( 'NONE', #7773, #10216, #1360 ) ;
#9728 = CARTESIAN_POINT ( 'NONE',  ( -2.293506896408097795, 80.56966535057935630, 16.00000000000000711 ) ) ;
#9729 = CARTESIAN_POINT ( 'NONE',  ( -56.36957570605425616, 90.52895752738122326, 10.90000000000000036 ) ) ;
#9730 = CARTESIAN_POINT ( 'NONE',  ( 37.60403889007154987, -135.1346877209587376, -26.91386751108004560 ) ) ;
#9731 = AXIS2_PLACEMENT_3D ( 'NONE', #3848, #4580, #2310 ) ;
#9732 = CARTESIAN_POINT ( 'NONE',  ( -30.29350689640809335, 120.5696653505793705, -16.00000000000000711 ) ) ;
#9733 = DIRECTION ( 'NONE',  ( 0.000000000000000000, 0.000000000000000000, -1.000000000000000000 ) ) ;
#9734 = ITEM_DEFINED_TRANSFORMATION ( 'NONE', 'NONE', #4300,  #4601 ) ;
#9735 = ORIENTED_EDGE ( 'NONE', *, *, #9022, .T. ) ;
#9736 = CARTESIAN_POINT ( 'NONE',  ( -56.36957570605427037, 137.0132282531173473, -4.025000000000000355 ) ) ;
#9737 = ADVANCED_FACE ( 'NONE', ( #152 ), #3378, .F. ) ;
#9738 = EDGE_LOOP ( 'NONE', ( #9792, #10273, #1755 ) ) ;
#9739 = VECTOR ( 'NONE', #10242, 1000.000000000000000 ) ;
#9740 = VERTEX_POINT ( 'NONE', #3322 ) ;
#9741 = DIRECTION ( 'NONE',  ( -0.000000000000000000, -0.000000000000000000, -1.000000000000000000 ) ) ;
#9742 = AXIS2_PLACEMENT_3D ( 'NONE', #8747, #739, #7209 ) ;
#9743 = DIRECTION ( 'NONE',  ( 0.000000000000000000, 0.000000000000000000, 1.000000000000000000 ) ) ;
#9744 = CARTESIAN_POINT ( 'NONE',  ( -164.8502026021585607, 257.7787449950629934, 0.000000000000000000 ) ) ;
#9745 = ADVANCED_BREP_SHAPE_REPRESENTATION ( '', ( #9837, #4601 ), #9559 ) ;
#9746 = CARTESIAN_POINT ( 'NONE',  ( -30.29350689640809335, 120.5696653505793705, 20.00000000000000711 ) ) ;
#9747 = CARTESIAN_POINT ( 'NONE',  ( 0.3000000000000016542, 0.000000000000000000, 4.700000000000000178 ) ) ;
#9748 = ORIENTED_EDGE ( 'NONE', *, *, #5173, .F. ) ;
#9749 = AXIS2_PLACEMENT_3D ( 'NONE', #7101, #1424, #1531 ) ;
#9750 = LINE ( 'NONE', #5702, #636 ) ;
#9751 = EDGE_CURVE ( 'NONE', #3286, #3513, #8089, .T. ) ;
#9752 = ADVANCED_FACE ( 'NONE', ( #830 ), #5763, .F. ) ;
#9753 = ORIENTED_EDGE ( 'NONE', *, *, #9751, .F. ) ;
#9754 = FACE_OUTER_BOUND ( 'NONE', #9319, .T. ) ;
#9755 = DIRECTION ( 'NONE',  ( 0.000000000000000000, 0.000000000000000000, -1.000000000000000000 ) ) ;
#9756 = CIRCLE ( 'NONE', #9933, 8.855570079111213744 ) ;
#9757 = LINE ( 'NONE', #7260, #4053 ) ;
#9758 = DIRECTION ( 'NONE',  ( 0.000000000000000000, 0.000000000000000000, 1.000000000000000000 ) ) ;
#9759 = CARTESIAN_POINT ( 'NONE',  ( 3.000000000000000000, 0.000000000000000000, 0.000000000000000000 ) ) ;
#9760 = TOROIDAL_SURFACE ( 'NONE', #1281, -39.11828581851394659, 47.56532671630426989 ) ;
#9761 = DIRECTION ( 'NONE',  ( 0.000000000000000000, 0.000000000000000000, 1.000000000000000000 ) ) ;
#9762 = ORIENTED_EDGE ( 'NONE', *, *, #3802, .F. ) ;
#9763 = ORIENTED_EDGE ( 'NONE', *, *, #5847, .T. ) ;
#9764 = ORIENTED_EDGE ( 'NONE', *, *, #8919, .F. ) ;
#9765 = AXIS2_PLACEMENT_3D ( 'NONE', #5231, #7725, #6823 ) ;
#9766 = ADVANCED_FACE ( 'NONE', ( #4066 ), #7352, .F. ) ;
#9767 = CIRCLE ( 'NONE', #3492, 4.024999999999997691 ) ;
#9768 = ORIENTED_EDGE ( 'NONE', *, *, #1542, .T. ) ;
#9769 = EDGE_CURVE ( 'NONE', #6079, #1518, #2556, .T. ) ;
#9770 = DIRECTION ( 'NONE',  ( 0.000000000000000000, 1.000000000000000000, -1.329743448921560837E-15 ) ) ;
#9771 = FILL_AREA_STYLE_COLOUR ( '', #1042 ) ;
#9772 = FACE_OUTER_BOUND ( 'NONE', #7850, .T. ) ;
#9773 = DIRECTION ( 'NONE',  ( 0.000000000000000000, 0.000000000000000000, 1.000000000000000000 ) ) ;
#9774 = AXIS2_PLACEMENT_3D ( 'NONE', #5575, #7915, #8759 ) ;
#9775 = ORIENTED_EDGE ( 'NONE', *, *, #1902, .F. ) ;
#9776 = DIRECTION ( 'NONE',  ( 1.000000000000000000, 0.000000000000000000, 0.000000000000000000 ) ) ;
#9777 = CIRCLE ( 'NONE', #1093, 2.000000000000001776 ) ;
#9778 = VERTEX_POINT ( 'NONE', #4851 ) ;
#9779 = AXIS2_PLACEMENT_3D ( 'NONE', #876, #8192, #4848 ) ;
#9780 = CARTESIAN_POINT ( 'NONE',  ( 37.22511195853866894, 17.84145331825995839, 25.00000000000000000 ) ) ;
#9781 = VECTOR ( 'NONE', #3971, 1000.000000000000000 ) ;
#9782 = ORIENTED_EDGE ( 'NONE', *, *, #2944, .T. ) ;
#9783 = VERTEX_POINT ( 'NONE', #2470 ) ;
#9784 = LINE ( 'NONE', #9835, #1153 ) ;
#9785 = DIRECTION ( 'NONE',  ( -1.000000000000000000, -0.000000000000000000, -0.000000000000000000 ) ) ;
#9786 = CARTESIAN_POINT ( 'NONE',  ( -16.29350689640809691, -19.43033464942062238, 7.500000000000000000 ) ) ;
#9787 = DIRECTION ( 'NONE',  ( -0.000000000000000000, -0.000000000000000000, -1.000000000000000000 ) ) ;
#9788 = EDGE_CURVE ( 'NONE', #5030, #3054, #2635, .T. ) ;
#9789 = DIRECTION ( 'NONE',  ( 1.000000000000000000, 0.000000000000000000, 0.000000000000000000 ) ) ;
#9790 = ORIENTED_EDGE ( 'NONE', *, *, #10101, .F. ) ;
#9791 = LINE ( 'NONE', #2405, #6815 ) ;
#9792 = ORIENTED_EDGE ( 'NONE', *, *, #4801, .F. ) ;
#9793 = DIRECTION ( 'NONE',  ( 6.982941293900105430E-16, -0.000000000000000000, -1.000000000000000000 ) ) ;
#9794 = VERTEX_POINT ( 'NONE', #7297 ) ;
#9795 = AXIS2_PLACEMENT_3D ( 'NONE', #7047, #10285, #9486 ) ;
#9796 = VECTOR ( 'NONE', #2024, 1000.000000000000000 ) ;
#9797 =( REPRESENTATION_RELATIONSHIP ('NONE','NONE', #9007, #5068 ) REPRESENTATION_RELATIONSHIP_WITH_TRANSFORMATION ( #1565 )SHAPE_REPRESENTATION_RELATIONSHIP( ) );
#9798 = DIRECTION ( 'NONE',  ( 0.000000000000000000, 0.000000000000000000, 1.000000000000000000 ) ) ;
#9799 = CARTESIAN_POINT ( 'NONE',  ( -40.00000000000001421, -135.1457019118818721, -40.00000000000002132 ) ) ;
#9800 = DIRECTION ( 'NONE',  ( 0.000000000000000000, -1.000000000000000000, 0.000000000000000000 ) ) ;
#9801 = DIRECTION ( 'NONE',  ( 0.000000000000000000, 1.460512169908342690E-16, -1.000000000000000000 ) ) ;
#9802 = DIRECTION ( 'NONE',  ( -0.000000000000000000, 0.000000000000000000, -1.000000000000000000 ) ) ;
#9803 = ADVANCED_FACE ( 'NONE', ( #1835 ), #4914, .T. ) ;
#9804 = CIRCLE ( 'NONE', #1497, 2.000000000000001776 ) ;
#9805 = ORIENTED_EDGE ( 'NONE', *, *, #5317, .T. ) ;
#9806 = CARTESIAN_POINT ( 'NONE',  ( -20.29350689640809691, 140.5696653505793563, -10.98204862120179648 ) ) ;
#9807 = AXIS2_PLACEMENT_3D ( 'NONE', #1522, #3258, #1568 ) ;
#9808 = VERTEX_POINT ( 'NONE', #6711 ) ;
#9809 = CARTESIAN_POINT ( 'NONE',  ( 3.000000000000000000, -1.467624384280024730, 2.542000000000003368 ) ) ;
#9810 = DIRECTION ( 'NONE',  ( 0.000000000000000000, -1.460512169908342690E-16, -1.000000000000000000 ) ) ;
#9811 = DIRECTION ( 'NONE',  ( 0.000000000000000000, -1.000000000000000000, 0.000000000000000000 ) ) ;
#9812 = LINE ( 'NONE', #9918, #9373 ) ;
#9813 = CARTESIAN_POINT ( 'NONE',  ( -2.293506896408097795, 37.08684478514406635, 25.00000000000000000 ) ) ;
#9814 = DIRECTION ( 'NONE',  ( 0.000000000000000000, -0.000000000000000000, -1.000000000000000000 ) ) ;
#9815 = AXIS2_PLACEMENT_3D ( 'NONE', #3631, #9248, #504 ) ;
#9816 = VERTEX_POINT ( 'NONE', #4954 ) ;
#9817 = EDGE_CURVE ( 'NONE', #2923, #9462, #6498, .T. ) ;
#9818 = ORIENTED_EDGE ( 'NONE', *, *, #10466, .F. ) ;
#9819 = ORIENTED_EDGE ( 'NONE', *, *, #1007, .T. ) ;
#9820 = EDGE_LOOP ( 'NONE', ( #1071, #9848, #6089, #4246, #1069 ) ) ;
#9821 = VECTOR ( 'NONE', #839, 1000.000000000000000 ) ;
#9822 = DIRECTION ( 'NONE',  ( 0.000000000000000000, 1.000000000000000000, -0.000000000000000000 ) ) ;
#9823 = LINE ( 'NONE', #2013, #2736 ) ;
#9824 = DIRECTION ( 'NONE',  ( -0.000000000000000000, -1.000000000000000000, -0.000000000000000000 ) ) ;
#9825 = DIRECTION ( 'NONE',  ( 0.08084652178105142251, -0.9929337167712581902, 0.08687044385014237868 ) ) ;
#9826 = EDGE_CURVE ( 'NONE', #4373, #3827, #1877, .T. ) ;
#9827 = CARTESIAN_POINT ( 'NONE',  ( 0.000000000000000000, 2.935248768560057897, -3.252606517456513302E-15 ) ) ;
#9828 = ADVANCED_FACE ( 'NONE', ( #8941 ), #8249, .T. ) ;
#9829 = EDGE_CURVE ( 'NONE', #2596, #1304, #3230, .T. ) ;
#9830 = EDGE_LOOP ( 'NONE', ( #9207, #88, #8530, #6048 ) ) ;
#9831 = CARTESIAN_POINT ( 'NONE',  ( -97.04168628513711781, 208.6400276031560566, 0.000000000000000000 ) ) ;
#9832 = ORIENTED_EDGE ( 'NONE', *, *, #2964, .F. ) ;
#9833 = UNCERTAINTY_MEASURE_WITH_UNIT (LENGTH_MEASURE( 1.000000000000000082E-05 ), #1764, 'distance_accuracy_value', 'NONE');
#9834 = VERTEX_POINT ( 'NONE', #879 ) ;
#9835 = CARTESIAN_POINT ( 'NONE',  ( -23.79350689640809691, 120.5289575273812233, 54.43095569077609497 ) ) ;
#9836 = CARTESIAN_POINT ( 'NONE',  ( -30.29350689640809335, 80.56966535057935630, -20.00000000000000711 ) ) ;
#9837 = MANIFOLD_SOLID_BREP ( 'Revolve1', #7236 ) ;
#9838 = DIRECTION ( 'NONE',  ( 0.000000000000000000, -1.000000000000000000, -1.222897680782651224E-16 ) ) ;
#9839 = DIRECTION ( 'NONE',  ( -1.000000000000000000, 0.000000000000000000, 0.000000000000000000 ) ) ;
#9840 = CYLINDRICAL_SURFACE ( 'NONE', #5489, 2.000000000000001776 ) ;
#9841 = DIRECTION ( 'NONE',  ( -0.000000000000000000, 0.000000000000000000, 1.000000000000000000 ) ) ;
#9842 = ADVANCED_FACE ( 'NONE', ( #5267 ), #4119, .F. ) ;
#9843 = EDGE_LOOP ( 'NONE', ( #1600, #8621, #328 ) ) ;
#9844 = DIRECTION ( 'NONE',  ( -0.000000000000000000, 1.000000000000000000, -0.000000000000000000 ) ) ;
#9845 = CONTEXT_DEPENDENT_SHAPE_REPRESENTATION ( #7419, #7132 ) ;
#9846 = EDGE_LOOP ( 'NONE', ( #820, #1438, #6312, #7459, #4465, #1341, #9725, #3244 ) ) ;
#9847 = DIRECTION ( 'NONE',  ( -0.000000000000000000, 1.000000000000000000, -0.000000000000000000 ) ) ;
#9848 = ORIENTED_EDGE ( 'NONE', *, *, #5909, .F. ) ;
#9849 = EDGE_CURVE ( 'NONE', #8972, #4758, #10361, .T. ) ;
#9850 = DIRECTION ( 'NONE',  ( 1.000000000000000000, 0.000000000000000000, 0.000000000000000000 ) ) ;
#9851 = VECTOR ( 'NONE', #95, 1000.000000000000000 ) ;
#9852 = CARTESIAN_POINT ( 'NONE',  ( -40.00000000000001421, -145.1457019118819005, -44.00000000000001421 ) ) ;
#9853 = DIRECTION ( 'NONE',  ( 0.000000000000000000, 0.000000000000000000, -1.000000000000000000 ) ) ;
#9854 = DIRECTION ( 'NONE',  ( 1.000000000000000000, 0.000000000000000000, 0.000000000000000000 ) ) ;
#9855 = CARTESIAN_POINT ( 'NONE',  ( -7.293506896408097795, 120.5696653505793705, 28.00000000000000355 ) ) ;
#9856 = ORIENTED_EDGE ( 'NONE', *, *, #3900, .T. ) ;
#9857 = AXIS2_PLACEMENT_3D ( 'NONE', #3334, #8894, #6564 ) ;
#9858 = DIRECTION ( 'NONE',  ( -0.7431448254773957984, 0.6691306063588564612, 0.000000000000000000 ) ) ;
#9859 = AXIS2_PLACEMENT_3D ( 'NONE', #9201, #5167, #7662 ) ;
#9860 = ADVANCED_FACE ( 'NONE', ( #7713 ), #8456, .F. ) ;
#9861 = EDGE_LOOP ( 'NONE', ( #976, #3978 ) ) ;
#9862 = LINE ( 'NONE', #4231, #491 ) ;
#9863 = CARTESIAN_POINT ( 'NONE',  ( 53.40242741783141156, 42.08684478514406635, 25.00000000000000000 ) ) ;
#9864 = DIRECTION ( 'NONE',  ( 0.000000000000000000, -1.000000000000000000, 1.222897680782651224E-16 ) ) ;
#9865 = CARTESIAN_POINT ( 'NONE',  ( -39.00000000000000000, 3.117691453623999909, -1.799999999999972733 ) ) ;
#9866 = DIRECTION ( 'NONE',  ( -1.000000000000000000, -0.000000000000000000, -0.000000000000000000 ) ) ;
#9867 = CARTESIAN_POINT ( 'NONE',  ( -16.29350689640809691, -140.1746510883711778, 27.01918567566963247 ) ) ;
#9868 = VECTOR ( 'NONE', #65, 1000.000000000000000 ) ;
#9869 = VERTEX_POINT ( 'NONE', #8509 ) ;
#9870 = ORIENTED_EDGE ( 'NONE', *, *, #2171, .F. ) ;
#9871 = CIRCLE ( 'NONE', #9355, 7.999999999999994671 ) ;
#9872 = ORIENTED_EDGE ( 'NONE', *, *, #4331, .T. ) ;
#9873 = VECTOR ( 'NONE', #1564, 1000.000000000000000 ) ;
#9874 = EDGE_CURVE ( 'NONE', #34, #8144, #6763, .T. ) ;
#9875 = DIRECTION ( 'NONE',  ( 0.1124875939035004796, -0.07750954751059241365, -0.9906254646749721449 ) ) ;
#9876 = DIRECTION ( 'NONE',  ( 0.000000000000000000, 0.000000000000000000, 1.000000000000000000 ) ) ;
#9877 = DIRECTION ( 'NONE',  ( -1.000000000000000000, -0.000000000000000000, -0.000000000000000000 ) ) ;
#9878 = CARTESIAN_POINT ( 'NONE',  ( 39.99999999999997158, -135.1457019118818721, 39.99999999999997868 ) ) ;
#9879 = ORIENTED_EDGE ( 'NONE', *, *, #101, .T. ) ;
#9880 = DIRECTION ( 'NONE',  ( 0.000000000000000000, 0.000000000000000000, 1.000000000000000000 ) ) ;
#9881 = AXIS2_PLACEMENT_3D ( 'NONE', #1224, #6092, #5245 ) ;
#9882 = ORIENTED_EDGE ( 'NONE', *, *, #9964, .F. ) ;
#9883 = CARTESIAN_POINT ( 'NONE',  ( -2.293506896408097795, 120.5696653505793705, -20.00000000000000711 ) ) ;
#9884 = VERTEX_POINT ( 'NONE', #8352 ) ;
#9885 = EDGE_CURVE ( 'NONE', #8325, #723, #7811, .T. ) ;
#9886 = DIRECTION ( 'NONE',  ( 0.000000000000000000, 1.000000000000000000, 0.000000000000000000 ) ) ;
#9887 = EDGE_CURVE ( 'NONE', #6927, #9202, #2896, .T. ) ;
#9888 = CARTESIAN_POINT ( 'NONE',  ( -101.9861939659648726, 222.5115114232797282, 8.572527594031516577E-16 ) ) ;
#9889 = CIRCLE ( 'NONE', #2934, 1.999999999999998224 ) ;
#9890 = EDGE_CURVE ( 'NONE', #7087, #2784, #6012, .T. ) ;
#9891 = CARTESIAN_POINT ( 'NONE',  ( -31.74999999999995737, 0.000000000000000000, 3.000000000000000444 ) ) ;
#9892 = DIRECTION ( 'NONE',  ( -0.000000000000000000, 1.000000000000000000, 0.000000000000000000 ) ) ;
#9893 = EDGE_CURVE ( 'NONE', #7867, #6696, #6841, .T. ) ;
#9894 = CARTESIAN_POINT ( 'NONE',  ( -40.00000000000001421, -135.1457019118818721, -40.00000000000002132 ) ) ;
#9895 = DIRECTION ( 'NONE',  ( 0.000000000000000000, -1.000000000000000000, 1.222897680782651224E-16 ) ) ;
#9896 = ORIENTED_EDGE ( 'NONE', *, *, #9517, .T. ) ;
#9897 = CARTESIAN_POINT ( 'NONE',  ( 18.34874108452142494, -140.1746510883711778, -97.78965767959371647 ) ) ;
#9898 = CIRCLE ( 'NONE', #7857, 4.000000000000000000 ) ;
#9899 = ORIENTED_EDGE ( 'NONE', *, *, #9379, .T. ) ;
#9900 =( GEOMETRIC_REPRESENTATION_CONTEXT ( 3 ) GLOBAL_UNCERTAINTY_ASSIGNED_CONTEXT ( ( #6532 ) ) GLOBAL_UNIT_ASSIGNED_CONTEXT ( ( #9441, #9551, #1378 ) ) REPRESENTATION_CONTEXT ( 'NONE', 'WORKASPACE' ) );
#9901 = FACE_OUTER_BOUND ( 'NONE', #3627, .T. ) ;
#9902 = EDGE_LOOP ( 'NONE', ( #5085, #7653, #6677, #2672 ) ) ;
#9903 = ADVANCED_FACE ( 'NONE', ( #5119 ), #3637, .T. ) ;
#9904 = VECTOR ( 'NONE', #2467, 1000.000000000000000 ) ;
#9905 = FACE_OUTER_BOUND ( 'NONE', #4790, .T. ) ;
#9906 = DIRECTION ( 'NONE',  ( -1.000000000000000000, 0.000000000000000000, 0.000000000000000000 ) ) ;
#9907 = DIRECTION ( 'NONE',  ( 0.000000000000000000, -1.000000000000000000, 0.000000000000000000 ) ) ;
#9908 = ORIENTED_EDGE ( 'NONE', *, *, #6715, .T. ) ;
#9909 = PRESENTATION_STYLE_ASSIGNMENT (( #7403 ) ) ;
#9910 = CARTESIAN_POINT ( 'NONE',  ( 0.000000000000000000, 0.000000000000000000, 4.700000000000000178 ) ) ;
#9911 = VERTEX_POINT ( 'NONE', #2039 ) ;
#9912 = AXIS2_PLACEMENT_3D ( 'NONE', #3305, #8074, #1667 ) ;
#9913 = DIRECTION ( 'NONE',  ( -1.000000000000000000, 0.000000000000000000, 0.000000000000000000 ) ) ;
#9914 = CIRCLE ( 'NONE', #8548, 3.999999999999996447 ) ;
#9915 = VERTEX_POINT ( 'NONE', #3695 ) ;
#9916 = DIRECTION ( 'NONE',  ( 1.000000000000000000, -7.780263845122167369E-16, 0.000000000000000000 ) ) ;
#9917 = FACE_BOUND ( 'NONE', #1570, .T. ) ;
#9918 = CARTESIAN_POINT ( 'NONE',  ( -23.79350689640809335, 76.32362273389503571, 54.43095569077609497 ) ) ;
#9919 = DIRECTION ( 'NONE',  ( 0.000000000000000000, -0.000000000000000000, -1.000000000000000000 ) ) ;
#9920 = DIRECTION ( 'NONE',  ( 0.000000000000000000, -1.000000000000000000, 1.329743448921560837E-15 ) ) ;
#9921 = ADVANCED_FACE ( 'NONE', ( #6924 ), #10159, .F. ) ;
#9922 = CIRCLE ( 'NONE', #763, 7.500000000000000000 ) ;
#9923 = ORIENTED_EDGE ( 'NONE', *, *, #678, .T. ) ;
#9924 = VERTEX_POINT ( 'NONE', #5908 ) ;
#9925 = VERTEX_POINT ( 'NONE', #9888 ) ;
#9926 = DIRECTION ( 'NONE',  ( -0.000000000000000000, -0.000000000000000000, 1.000000000000000000 ) ) ;
#9927 = CARTESIAN_POINT ( 'NONE',  ( 4.856471286862176662, 145.0444252872335937, 25.00000000000000000 ) ) ;
#9928 = AXIS2_PLACEMENT_3D ( 'NONE', #6226, #2201, #667 ) ;
#9929 = CARTESIAN_POINT ( 'NONE',  ( 26.00000000000000355, 0.000000000000000000, 2.445500000000000007 ) ) ;
#9930 = DIRECTION ( 'NONE',  ( 1.000000000000000000, 0.000000000000000000, -0.000000000000000000 ) ) ;
#9931 = EDGE_LOOP ( 'NONE', ( #2365, #2758, #2717, #6464, #9700 ) ) ;
#9932 = CARTESIAN_POINT ( 'NONE',  ( -2.293506896408097795, 37.08684478514406635, -25.00000000000000355 ) ) ;
#9933 = AXIS2_PLACEMENT_3D ( 'NONE', #4648, #5549, #6287 ) ;
#9934 = ORIENTED_EDGE ( 'NONE', *, *, #10252, .F. ) ;
#9935 = EDGE_CURVE ( 'NONE', #7686, #3419, #8335, .T. ) ;
#9936 = AXIS2_PLACEMENT_3D ( 'NONE', #6471, #9018, #8915 ) ;
#9937 = EDGE_LOOP ( 'NONE', ( #8486, #9017, #2891, #10290, #7650 ) ) ;
#9938 = UNCERTAINTY_MEASURE_WITH_UNIT (LENGTH_MEASURE( 1.000000000000000082E-05 ), #411, 'distance_accuracy_value', 'NONE');
#9939 = VERTEX_POINT ( 'NONE', #7333 ) ;
#9940 = CARTESIAN_POINT ( 'NONE',  ( -40.00000000000002842, -145.1457019118819005, 39.99999999999997868 ) ) ;
#9941 = FACE_OUTER_BOUND ( 'NONE', #6737, .T. ) ;
#9942 = VECTOR ( 'NONE', #6961, 1000.000000000000000 ) ;
#9943 = MANIFOLD_SOLID_BREP ( 'Cut-Extrude9', #2494 ) ;
#9944 = CARTESIAN_POINT ( 'NONE',  ( -8.793506896408096907, 120.5289575273812233, 54.43095569077609497 ) ) ;
#9945 = LINE ( 'NONE', #3410, #7989 ) ;
#9946 = FACE_OUTER_BOUND ( 'NONE', #5027, .T. ) ;
#9947 = DIRECTION ( 'NONE',  ( 0.000000000000000000, -1.000000000000000000, 0.000000000000000000 ) ) ;
#9948 = VERTEX_POINT ( 'NONE', #8283 ) ;
#9949 = DIRECTION ( 'NONE',  ( -1.000000000000000000, -0.000000000000000000, -0.000000000000000000 ) ) ;
#9950 = EDGE_CURVE ( 'NONE', #5946, #7078, #6690, .T. ) ;
#9951 = EDGE_CURVE ( 'NONE', #5556, #4617, #4934, .T. ) ;
#9952 = ORIENTED_EDGE ( 'NONE', *, *, #7993, .F. ) ;
#9953 = LINE ( 'NONE', #6754, #8607 ) ;
#9954 = VECTOR ( 'NONE', #10048, 1000.000000000000000 ) ;
#9955 = VERTEX_POINT ( 'NONE', #5893 ) ;
#9956 = CIRCLE ( 'NONE', #3342, 4.000000000000000000 ) ;
#9957 = DIRECTION ( 'NONE',  ( 0.000000000000000000, -0.000000000000000000, 1.000000000000000000 ) ) ;
#9958 = CARTESIAN_POINT ( 'NONE',  ( 37.23846126345171825, -134.0500961303746692, 25.36885565376192275 ) ) ;
#9959 = LINE ( 'NONE', #10104, #3144 ) ;
#9960 = DIRECTION ( 'NONE',  ( 0.000000000000000000, 0.000000000000000000, 1.000000000000000000 ) ) ;
#9961 = CIRCLE ( 'NONE', #2162, 5.000000000000000888 ) ;
#9962 = CARTESIAN_POINT ( 'NONE',  ( -7.293506896408097795, 112.5696653505793705, -20.00000000000000711 ) ) ;
#9963 = ADVANCED_FACE ( 'NONE', ( #9941 ), #8230, .F. ) ;
#9964 = EDGE_CURVE ( 'NONE', #9083, #9176, #5100, .T. ) ;
#9965 = ADVANCED_FACE ( 'NONE', ( #8175 ), #3462, .F. ) ;
#9966 = ORIENTED_EDGE ( 'NONE', *, *, #5833, .F. ) ;
#9967 = VECTOR ( 'NONE', #5303, 1000.000000000000000 ) ;
#9968 = FACE_OUTER_BOUND ( 'NONE', #1693, .T. ) ;
#9969 = ORIENTED_EDGE ( 'NONE', *, *, #300, .F. ) ;
#9970 = CARTESIAN_POINT ( 'NONE',  ( -2.293506896408097795, 55.56966535057937051, -10.98204862120179826 ) ) ;
#9971 = DIRECTION ( 'NONE',  ( 1.000000000000000000, -0.000000000000000000, -0.000000000000000000 ) ) ;
#9972 = PLANE ( 'NONE',  #5578 ) ;
#9973 = DIRECTION ( 'NONE',  ( -0.000000000000000000, 1.000000000000000000, 0.000000000000000000 ) ) ;
#9974 = DIRECTION ( 'NONE',  ( -0.000000000000000000, 1.000000000000000000, -0.000000000000000000 ) ) ;
#9975 = CIRCLE ( 'NONE', #325, 4.024999999999997691 ) ;
#9976 = DIRECTION ( 'NONE',  ( 0.000000000000000000, 0.000000000000000000, -1.000000000000000000 ) ) ;
#9977 = EDGE_CURVE ( 'NONE', #9437, #9023, #5838, .T. ) ;
#9978 = ORIENTED_EDGE ( 'NONE', *, *, #7022, .T. ) ;
#9979 = DIRECTION ( 'NONE',  ( -1.000000000000000000, 0.000000000000000000, 0.000000000000000000 ) ) ;
#9980 = EDGE_CURVE ( 'NONE', #4386, #6270, #5771, .T. ) ;
#9981 =( NAMED_UNIT ( * ) SI_UNIT ( $, .STERADIAN. ) SOLID_ANGLE_UNIT ( ) );
#9982 = CIRCLE ( 'NONE', #9465, 7.728925574020641953 ) ;
#9983 = DIRECTION ( 'NONE',  ( 1.000000000000000000, -0.000000000000000000, -0.000000000000000000 ) ) ;
#9984 = CARTESIAN_POINT ( 'NONE',  ( 6.000000000000005329, 0.000000000000000000, -3.250000000000000444 ) ) ;
#9985 = ORIENTED_EDGE ( 'NONE', *, *, #2247, .T. ) ;
#9986 = CARTESIAN_POINT ( 'NONE',  ( -25.15769640663940621, -135.1457019118818721, 27.15769640663938489 ) ) ;
#9987 = VERTEX_POINT ( 'NONE', #4206 ) ;
#9988 =( NAMED_UNIT ( * ) PLANE_ANGLE_UNIT ( ) SI_UNIT ( $, .RADIAN. ) );
#9989 = AXIS2_PLACEMENT_3D ( 'NONE', #2020, #8383, #1017 ) ;
#9990 = ORIENTED_EDGE ( 'NONE', *, *, #3042, .F. ) ;
#9991 = DIRECTION ( 'NONE',  ( 0.000000000000000000, 0.000000000000000000, -1.000000000000000000 ) ) ;
#9992 = PRESENTATION_STYLE_ASSIGNMENT (( #6744 ) ) ;
#9993 = CARTESIAN_POINT ( 'NONE',  ( -11.29350689640809158, 105.5289575273812233, 7.749999999999999112 ) ) ;
#9994 = CARTESIAN_POINT ( 'NONE',  ( 37.22759939293836595, -133.1457019118818721, -25.15769640663939910 ) ) ;
#9995 = CARTESIAN_POINT ( 'NONE',  ( 0.000000000000000000, -115.1457019118818863, 47.99999999999997868 ) ) ;
#9996 = CARTESIAN_POINT ( 'NONE',  ( -47.94539818030330025, 137.0132282531173473, 3.999999999999991562 ) ) ;
#9997 = ORIENTED_EDGE ( 'NONE', *, *, #1006, .T. ) ;
#9998 = LINE ( 'NONE', #2718, #8681 ) ;
#9999 = ORIENTED_EDGE ( 'NONE', *, *, #1594, .T. ) ;
#10000 = DIRECTION ( 'NONE',  ( 1.000000000000000000, -0.000000000000000000, -0.000000000000000000 ) ) ;
#10001 = ORIENTED_EDGE ( 'NONE', *, *, #8171, .F. ) ;
#10002 = EDGE_CURVE ( 'NONE', #2498, #6206, #4988, .T. ) ;
#10003 = PLANE ( 'NONE',  #3337 ) ;
#10004 = CARTESIAN_POINT ( 'NONE',  ( 37.22797402574886405, -133.4133323156204654, 25.17121823815657677 ) ) ;
#10005 = CARTESIAN_POINT ( 'NONE',  ( -56.34457570605425758, 137.0132282531173473, 0.000000000000000000 ) ) ;
#10006 = ORIENTED_EDGE ( 'NONE', *, *, #7902, .F. ) ;
#10007 = DIRECTION ( 'NONE',  ( -0.000000000000000000, 0.000000000000000000, 1.000000000000000000 ) ) ;
#10008 = CARTESIAN_POINT ( 'NONE',  ( -20.29350689640809691, 140.5696653505793847, -22.32382185646122963 ) ) ;
#10009 = ORIENTED_EDGE ( 'NONE', *, *, #1687, .F. ) ;
#10010 = FACE_OUTER_BOUND ( 'NONE', #9420, .T. ) ;
#10011 = ORIENTED_EDGE ( 'NONE', *, *, #8597, .F. ) ;
#10012 = FACE_OUTER_BOUND ( 'NONE', #8060, .T. ) ;
#10013 = EDGE_CURVE ( 'NONE', #3513, #640, #4151, .T. ) ;
#10014 = CARTESIAN_POINT ( 'NONE',  ( -2.293506896408097795, 120.5696653505793705, -20.00000000000000711 ) ) ;
#10015 = ADVANCED_FACE ( 'NONE', ( #9026, #7439, #2508, #2712 ), #2615, .F. ) ;
#10016 = ADVANCED_FACE ( 'NONE', ( #445 ), #6285, .F. ) ;
#10017 = CARTESIAN_POINT ( 'NONE',  ( -27.15769640663940621, -135.1457019118818721, -3.792811993702496405E-15 ) ) ;
#10018 = CARTESIAN_POINT ( 'NONE',  ( -20.29350689640809691, 140.5696653505793563, 10.90000000000000036 ) ) ;
#10019 = CARTESIAN_POINT ( 'NONE',  ( -18.34874108452141783, -140.1746510883711778, 29.59847408863694440 ) ) ;
#10020 = CARTESIAN_POINT ( 'NONE',  ( -38.96131932220313132, -3.592756407884938330, -1.758437202063725779 ) ) ;
#10021 = VECTOR ( 'NONE', #7549, 1000.000000000000000 ) ;
#10022 = ORIENTED_EDGE ( 'NONE', *, *, #9396, .T. ) ;
#10023 = VERTEX_POINT ( 'NONE', #544 ) ;
#10024 = CARTESIAN_POINT ( 'NONE',  ( -3.173844575093148990, 150.5696653505793563, -10.90000000000000036 ) ) ;
#10025 = ADVANCED_FACE ( 'NONE', ( #1343 ), #2076, .T. ) ;
#10026 = VECTOR ( 'NONE', #3664, 1000.000000000000000 ) ;
#10027 = LINE ( 'NONE', #10134, #9547 ) ;
#10028 = CARTESIAN_POINT ( 'NONE',  ( -7.293506896408097795, 4.007378841484243628E-15, 28.00000000000002132 ) ) ;
#10029 = ORIENTED_EDGE ( 'NONE', *, *, #1293, .F. ) ;
#10030 = DIRECTION ( 'NONE',  ( -0.000000000000000000, 1.000000000000000000, -0.000000000000000000 ) ) ;
#10031 = ORIENTED_EDGE ( 'NONE', *, *, #2245, .F. ) ;
#10032 = AXIS2_PLACEMENT_3D ( 'NONE', #4545, #6288, #3247 ) ;
#10033 = EDGE_LOOP ( 'NONE', ( #764, #10244, #4530 ) ) ;
#10034 = CARTESIAN_POINT ( 'NONE',  ( 37.22759939293836595, -117.1457019118819005, -25.15769640663939910 ) ) ;
#10035 = DIRECTION ( 'NONE',  ( 1.137729606058012035E-16, 0.000000000000000000, 1.000000000000000000 ) ) ;
#10036 = FACE_OUTER_BOUND ( 'NONE', #7597, .T. ) ;
#10037 = DIRECTION ( 'NONE',  ( 0.000000000000000000, 0.000000000000000000, -1.000000000000000000 ) ) ;
#10038 = AXIS2_PLACEMENT_3D ( 'NONE', #601, #8760, #3942 ) ;
#10039 = CARTESIAN_POINT ( 'NONE',  ( -16.29350689640809691, -8.660287962196477451, 6.499999999999964473 ) ) ;
#10040 = EDGE_LOOP ( 'NONE', ( #8513, #6097, #3698, #2920, #1201 ) ) ;
#10041 = DIRECTION ( 'NONE',  ( 0.000000000000000000, 0.7071067811864494290, 0.7071067811866454944 ) ) ;
#10042 = EDGE_CURVE ( 'NONE', #8095, #9794, #2871, .T. ) ;
#10043 = ORIENTED_EDGE ( 'NONE', *, *, #3733, .T. ) ;
#10044 = CIRCLE ( 'NONE', #6999, 19.24539146688411506 ) ;
#10045 = DIRECTION ( 'NONE',  ( -1.000000000000000000, 0.000000000000000000, 0.000000000000000000 ) ) ;
#10046 = ORIENTED_EDGE ( 'NONE', *, *, #5206, .T. ) ;
#10047 = APPLICATION_CONTEXT ( 'automotive_design' ) ;
#10048 = DIRECTION ( 'NONE',  ( 1.396588258780021135E-16, 0.000000000000000000, -1.000000000000000000 ) ) ;
#10049 = FACE_OUTER_BOUND ( 'NONE', #6755, .T. ) ;
#10050 = DIRECTION ( 'NONE',  ( 0.000000000000000000, 1.000000000000000000, 0.000000000000000000 ) ) ;
#10051 = CIRCLE ( 'NONE', #3274, 4.024999999999997691 ) ;
#10052 = ORIENTED_EDGE ( 'NONE', *, *, #3540, .T. ) ;
#10053 = DIRECTION ( 'NONE',  ( 0.000000000000000000, -1.734723475976808278E-15, 1.000000000000000000 ) ) ;
#10054 = ORIENTED_EDGE ( 'NONE', *, *, #3911, .T. ) ;
#10055 = DIRECTION ( 'NONE',  ( 1.000000000000000000, 0.000000000000000000, 0.000000000000000000 ) ) ;
#10056 = EDGE_CURVE ( 'NONE', #10372, #2017, #8547, .T. ) ;
#10057 = ORIENTED_EDGE ( 'NONE', *, *, #7804, .T. ) ;
#10058 = CARTESIAN_POINT ( 'NONE',  ( -56.36957570605426326, 90.52895752738122326, 10.90000000000000036 ) ) ;
#10059 = CIRCLE ( 'NONE', #742, 3.999999999999996447 ) ;
#10060 = ORIENTED_EDGE ( 'NONE', *, *, #2627, .F. ) ;
#10061 = DIRECTION ( 'NONE',  ( 1.000000000000000000, -9.013708445275205736E-16, 0.000000000000000000 ) ) ;
#10062 = CARTESIAN_POINT ( 'NONE',  ( -18.34874108452141783, -140.1746510883711778, -7.212905963064413228 ) ) ;
#10063 = CIRCLE ( 'NONE', #255, 7.500000000000000000 ) ;
#10064 = LINE ( 'NONE', #6772, #832 ) ;
#10065 = CARTESIAN_POINT ( 'NONE',  ( -2.293506896408097795, -0.3998014571812398832, -1.076388538564875708 ) ) ;
#10066 = CARTESIAN_POINT ( 'NONE',  ( 77.30044127146540234, 73.68369600860394542, 25.00000000000000000 ) ) ;
#10067 = DIRECTION ( 'NONE',  ( 1.000000000000000000, -0.000000000000000000, -0.000000000000000000 ) ) ;
#10068 = VECTOR ( 'NONE', #8926, 1000.000000000000000 ) ;
#10069 = VERTEX_POINT ( 'NONE', #9397 ) ;
#10070 = EDGE_CURVE ( 'NONE', #3513, #10220, #3075, .T. ) ;
#10071 = ORIENTED_EDGE ( 'NONE', *, *, #2681, .F. ) ;
#10072 = VECTOR ( 'NONE', #3526, 1000.000000000000000 ) ;
#10073 = ADVANCED_FACE ( 'NONE', ( #5252 ), #2818, .F. ) ;
#10074 = ADVANCED_FACE ( 'NONE', ( #6155, #6100, #9184 ), #5151, .F. ) ;
#10075 = CARTESIAN_POINT ( 'NONE',  ( -97.04168628513710360, 208.6400276031560281, 0.000000000000000000 ) ) ;
#10076 = EDGE_LOOP ( 'NONE', ( #6978, #2068, #5924, #4812 ) ) ;
#10077 = FACE_OUTER_BOUND ( 'NONE', #899, .T. ) ;
#10078 = SHAPE_REPRESENTATION_RELATIONSHIP ( 'NONE' , 'NONE' ,  #1081, #638 ) ;
#10079 = FACE_OUTER_BOUND ( 'NONE', #565, .T. ) ;
#10080 = DIRECTION ( 'NONE',  ( 0.000000000000000000, -1.000000000000000000, 1.431206729101514631E-16 ) ) ;
#10081 = VECTOR ( 'NONE', #2594, 1000.000000000000227 ) ;
#10082 = VERTEX_POINT ( 'NONE', #7755 ) ;
#10083 = ORIENTED_EDGE ( 'NONE', *, *, #10395, .T. ) ;
#10084 = FILL_AREA_STYLE_COLOUR ( '', #6930 ) ;
#10085 = PRODUCT_RELATED_PRODUCT_CATEGORY ( 'part', '', ( #5681 ) ) ;
#10086 = EDGE_CURVE ( 'NONE', #8738, #996, #3677, .T. ) ;
#10087 = EDGE_CURVE ( 'NONE', #5429, #4328, #2764, .T. ) ;
#10088 = ORIENTED_EDGE ( 'NONE', *, *, #3979, .F. ) ;
#10089 = FACE_OUTER_BOUND ( 'NONE', #9638, .T. ) ;
#10090 = CARTESIAN_POINT ( 'NONE',  ( -55.94539818030328604, 145.0132282531173189, -3.999999999999992895 ) ) ;
#10091 = CYLINDRICAL_SURFACE ( 'NONE', #7560, 5.000000000000001776 ) ;
#10092 = DIRECTION ( 'NONE',  ( -1.000000000000000000, 0.000000000000000000, 0.000000000000000000 ) ) ;
#10093 = AXIS2_PLACEMENT_3D ( 'NONE', #8976, #2616, #7543 ) ;
#10094 = CARTESIAN_POINT ( 'NONE',  ( -2.293506896408097795, 42.08684478514410188, -30.00000000000000355 ) ) ;
#10095 = ORIENTED_EDGE ( 'NONE', *, *, #10395, .F. ) ;
#10096 = DIRECTION ( 'NONE',  ( -7.061912783291096091E-17, 0.08715574274765486296, 0.9961946980917458783 ) ) ;
#10097 = VECTOR ( 'NONE', #4412, 1000.000000000000000 ) ;
#10098 = LINE ( 'NONE', #1294, #2014 ) ;
#10099 = FACE_OUTER_BOUND ( 'NONE', #9499, .T. ) ;
#10100 = AXIS2_PLACEMENT_3D ( 'NONE', #3943, #7126, #9347 ) ;
#10101 = EDGE_CURVE ( 'NONE', #5230, #3031, #1883, .T. ) ;
#10102 = DIRECTION ( 'NONE',  ( 0.000000000000000000, 1.000000000000000000, 0.000000000000000000 ) ) ;
#10103 = CARTESIAN_POINT ( 'NONE',  ( 14.70649310359190309, 80.56966535057935630, -20.00000000000000711 ) ) ;
#10104 = CARTESIAN_POINT ( 'NONE',  ( 32.59878849545336976, 32.08684478514406635, 30.00000000000000355 ) ) ;
#10105 = CIRCLE ( 'NONE', #8751, 9.050254677131414738 ) ;
#10106 =( NAMED_UNIT ( * ) SI_UNIT ( $, .STERADIAN. ) SOLID_ANGLE_UNIT ( ) );
#10107 = VERTEX_POINT ( 'NONE', #4363 ) ;
#10108 = CARTESIAN_POINT ( 'NONE',  ( 3.000000000000000000, 1.467624384280033167, 2.541999999999999371 ) ) ;
#10109 = VECTOR ( 'NONE', #4198, 1000.000000000000000 ) ;
#10110 = VECTOR ( 'NONE', #1461, 1000.000000000000114 ) ;
#10111 = ORIENTED_EDGE ( 'NONE', *, *, #5713, .F. ) ;
#10112 = CARTESIAN_POINT ( 'NONE',  ( 0.000000000000000000, 0.000000000000000000, 0.000000000000000000 ) ) ;
#10113 = ORIENTED_EDGE ( 'NONE', *, *, #3673, .F. ) ;
#10114 = LINE ( 'NONE', #3700, #3851 ) ;
#10115 = ORIENTED_EDGE ( 'NONE', *, *, #1772, .F. ) ;
#10116 = AXIS2_PLACEMENT_3D ( 'NONE', #8869, #1557, #7924 ) ;
#10117 = VERTEX_POINT ( 'NONE', #2926 ) ;
#10118 = CARTESIAN_POINT ( 'NONE',  ( 10.26554134690924691, 150.5696653505793563, 7.749999999999998224 ) ) ;
#10119 = DIRECTION ( 'NONE',  ( 0.000000000000000000, -1.000000000000000000, -1.431206729101514631E-16 ) ) ;
#10120 = VERTEX_POINT ( 'NONE', #2130 ) ;
#10121 = CARTESIAN_POINT ( 'NONE',  ( 37.71464122736488633, -135.1457019118818721, 27.15769640663938489 ) ) ;
#10122 = VECTOR ( 'NONE', #8164, 1000.000000000000000 ) ;
#10123 = CARTESIAN_POINT ( 'NONE',  ( -23.15769640663940976, -117.1457019118819005, 27.15769640663938489 ) ) ;
#10124 = DIRECTION ( 'NONE',  ( 0.000000000000000000, -1.000000000000000000, -0.000000000000000000 ) ) ;
#10125 = CARTESIAN_POINT ( 'NONE',  ( -121.1992630477586346, 230.3916074206559017, 0.000000000000000000 ) ) ;
#10126 = AXIS2_PLACEMENT_3D ( 'NONE', #8385, #9395, #543 ) ;
#10127 = ORIENTED_EDGE ( 'NONE', *, *, #6146, .F. ) ;
#10128 = ORIENTED_EDGE ( 'NONE', *, *, #7336, .T. ) ;
#10129 = CARTESIAN_POINT ( 'NONE',  ( -94.36516385970165288, 211.6126069050656042, 4.898587196589436495E-16 ) ) ;
#10130 = ORIENTED_EDGE ( 'NONE', *, *, #1656, .F. ) ;
#10131 = DIRECTION ( 'NONE',  ( -0.000000000000000000, 1.000000000000000000, -0.000000000000000000 ) ) ;
#10132 =( NAMED_UNIT ( * ) PLANE_ANGLE_UNIT ( ) SI_UNIT ( $, .RADIAN. ) );
#10133 = CIRCLE ( 'NONE', #1830, 9.050254677131414738 ) ;
#10134 = CARTESIAN_POINT ( 'NONE',  ( -30.29350689640809335, 128.5696653505793563, -20.00000000000000711 ) ) ;
#10135 = EDGE_CURVE ( 'NONE', #4046, #7873, #391, .T. ) ;
#10136 = DIRECTION ( 'NONE',  ( -1.000000000000000000, 0.000000000000000000, 0.000000000000000000 ) ) ;
#10137 = EDGE_LOOP ( 'NONE', ( #3972, #5952, #1100, #6517 ) ) ;
#10138 = ORIENTED_EDGE ( 'NONE', *, *, #6932, .F. ) ;
#10139 = ORIENTED_EDGE ( 'NONE', *, *, #757, .F. ) ;
#10140 = AXIS2_PLACEMENT_3D ( 'NONE', #5369, #4528, #8450 ) ;
#10141 = ORIENTED_EDGE ( 'NONE', *, *, #8171, .T. ) ;
#10142 = DIRECTION ( 'NONE',  ( 6.982941293900105430E-16, -0.000000000000000000, -1.000000000000000000 ) ) ;
#10143 = CARTESIAN_POINT ( 'NONE',  ( -47.94539818030330025, 90.52895752738122326, 3.999999999999993339 ) ) ;
#10144 = CYLINDRICAL_SURFACE ( 'NONE', #10382, 7.499999999999998224 ) ;
#10145 = EDGE_CURVE ( 'NONE', #426, #4585, #9292, .T. ) ;
#10146 = EDGE_CURVE ( 'NONE', #2699, #10120, #6625, .T. ) ;
#10147 = EDGE_CURVE ( 'NONE', #9529, #2275, #3406, .T. ) ;
#10148 = CARTESIAN_POINT ( 'NONE',  ( 32.59878849545336976, 32.08684478514406635, -12.49999999999999289 ) ) ;
#10149 = EDGE_LOOP ( 'NONE', ( #7637, #8755, #5387, #6954 ) ) ;
#10150 = VECTOR ( 'NONE', #9864, 1000.000000000000000 ) ;
#10151 = DIRECTION ( 'NONE',  ( 1.000000000000000000, -0.000000000000000000, -0.000000000000000000 ) ) ;
#10152 = CARTESIAN_POINT ( 'NONE',  ( -30.29350689640809335, 150.5696653505793563, 20.00000000000000355 ) ) ;
#10153 = ORIENTED_EDGE ( 'NONE', *, *, #1188, .T. ) ;
#10154 = VECTOR ( 'NONE', #7043, 1000.000000000000000 ) ;
#10155 = EDGE_CURVE ( 'NONE', #7686, #382, #10158, .T. ) ;
#10156 = LINE ( 'NONE', #1354, #4852 ) ;
#10157 = DIRECTION ( 'NONE',  ( -1.000000000000000000, 0.000000000000000000, -9.776117811460135374E-16 ) ) ;
#10158 =( BOUNDED_CURVE ( )  B_SPLINE_CURVE ( 3, ( #6852, #10090, #6050, #11 ),
 .UNSPECIFIED., .F., .F. ) 
 B_SPLINE_CURVE_WITH_KNOTS ( ( 4, 4 ),
 ( 4.712388980384689674, 7.853981633974482790 ),
 .UNSPECIFIED. ) 
 CURVE ( )  GEOMETRIC_REPRESENTATION_ITEM ( )  RATIONAL_B_SPLINE_CURVE ( ( 1.000000000000000000, 0.3333333333333333703, 0.3333333333333333703, 1.000000000000000000 ) ) 
 REPRESENTATION_ITEM ( '' )  );
#10159 = CYLINDRICAL_SURFACE ( 'NONE', #3932, 4.024999999999997691 ) ;
#10160 = ORIENTED_EDGE ( 'NONE', *, *, #7538, .T. ) ;
#10161 = DIRECTION ( 'NONE',  ( 0.000000000000000000, -1.000000000000000000, 0.000000000000000000 ) ) ;
#10162 = ORIENTED_EDGE ( 'NONE', *, *, #8389, .F. ) ;
#10163 = DIRECTION ( 'NONE',  ( 1.000000000000000000, 0.000000000000000000, 0.000000000000000000 ) ) ;
#10164 = VERTEX_POINT ( 'NONE', #7645 ) ;
#10165 = PLANE ( 'NONE',  #7392 ) ;
#10166 = VERTEX_POINT ( 'NONE', #9563 ) ;
#10167 = VERTEX_POINT ( 'NONE', #4038 ) ;
#10168 = CYLINDRICAL_SURFACE ( 'NONE', #9765, 10.00000000000000178 ) ;
#10169 = DIRECTION ( 'NONE',  ( -1.000000000000000000, -0.000000000000000000, -0.000000000000000000 ) ) ;
#10170 = EDGE_LOOP ( 'NONE', ( #7243, #8157, #9985, #7449, #4614 ) ) ;
#10171 = DIRECTION ( 'NONE',  ( 0.000000000000000000, 0.4999999999999985567, -0.8660254037844394848 ) ) ;
#10172 = DIRECTION ( 'NONE',  ( 0.000000000000000000, 1.000000000000000000, -0.000000000000000000 ) ) ;
#10173 = CARTESIAN_POINT ( 'NONE',  ( -16.29350689640809691, -140.1746510883711778, 23.72119897386845722 ) ) ;
#10174 = CARTESIAN_POINT ( 'NONE',  ( -11.29350689640808802, 105.5289575273812233, 7.749999999999999112 ) ) ;
#10175 = ORIENTED_EDGE ( 'NONE', *, *, #8882, .T. ) ;
#10176 = EDGE_CURVE ( 'NONE', #289, #723, #3940, .T. ) ;
#10177 = ORIENTED_EDGE ( 'NONE', *, *, #5334, .T. ) ;
#10178 = CARTESIAN_POINT ( 'NONE',  ( -2.293506896408097795, 55.56966535057937051, 10.98204862120179826 ) ) ;
#10179 = CIRCLE ( 'NONE', #2889, 5.000000000000000888 ) ;
#10180 = ORIENTED_EDGE ( 'NONE', *, *, #7467, .F. ) ;
#10181 = DIRECTION ( 'NONE',  ( 1.734723475976805319E-15, -0.000000000000000000, -1.000000000000000000 ) ) ;
#10182 = FACE_OUTER_BOUND ( 'NONE', #9861, .T. ) ;
#10183 = FACE_BOUND ( 'NONE', #3752, .T. ) ;
#10184 = DIRECTION ( 'NONE',  ( 1.000000000000000000, -0.000000000000000000, -0.000000000000000000 ) ) ;
#10185 = CARTESIAN_POINT ( 'NONE',  ( -1.071796769724492338, 4.898587196589411843E-16, -3.999999999999999112 ) ) ;
#10186 = AXIS2_PLACEMENT_3D ( 'NONE', #7491, #7383, #1285 ) ;
#10187 = VERTEX_POINT ( 'NONE', #749 ) ;
#10188 = ORIENTED_EDGE ( 'NONE', *, *, #6063, .F. ) ;
#10189 = EDGE_CURVE ( 'NONE', #4869, #4943, #8322, .T. ) ;
#10190 = AXIS2_PLACEMENT_3D ( 'NONE', #2987, #4627, #3879 ) ;
#10191 = ORIENTED_EDGE ( 'NONE', *, *, #7010, .T. ) ;
#10192 = CIRCLE ( 'NONE', #874, 1.999999999999998224 ) ;
#10193 = EDGE_LOOP ( 'NONE', ( #3897, #10272, #58, #8271 ) ) ;
#10194 = CARTESIAN_POINT ( 'NONE',  ( -134.8713710537857935, 257.7072748320279061, 1.365612337163390183E-15 ) ) ;
#10195 = DIRECTION ( 'NONE',  ( 0.000000000000000000, 0.000000000000000000, -1.000000000000000000 ) ) ;
#10196 = CARTESIAN_POINT ( 'NONE',  ( -2.293506896408097795, 120.5696653505793705, 20.00000000000000711 ) ) ;
#10197 = LINE ( 'NONE', #8762, #4341 ) ;
#10198 = AXIS2_PLACEMENT_3D ( 'NONE', #9078, #1024, #5895 ) ;
#10199 = ORIENTED_EDGE ( 'NONE', *, *, #251, .F. ) ;
#10200 = AXIS2_PLACEMENT_3D ( 'NONE', #1148, #4385, #6813 ) ;
#10201 = DIRECTION ( 'NONE',  ( 0.000000000000000000, 0.4999999999999985567, -0.8660254037844394848 ) ) ;
#10202 = EDGE_CURVE ( 'NONE', #898, #10372, #1553, .T. ) ;
#10203 = ADVANCED_FACE ( 'NONE', ( #10308, #3985 ), #656, .T. ) ;
#10204 = EDGE_CURVE ( 'NONE', #5617, #59, #7972, .T. ) ;
#10205 = DIRECTION ( 'NONE',  ( 0.000000000000000000, 0.000000000000000000, 1.000000000000000000 ) ) ;
#10206 = DIRECTION ( 'NONE',  ( -0.000000000000000000, -0.000000000000000000, -1.000000000000000000 ) ) ;
#10207 = CIRCLE ( 'NONE', #10038, 4.000000000000003553 ) ;
#10208 = CIRCLE ( 'NONE', #2754, 2.000000000000001776 ) ;
#10209 = DIRECTION ( 'NONE',  ( 1.000000000000000000, 0.000000000000000000, -0.000000000000000000 ) ) ;
#10210 = DIRECTION ( 'NONE',  ( 0.000000000000000000, 0.000000000000000000, 1.000000000000000000 ) ) ;
#10211 = CYLINDRICAL_SURFACE ( 'NONE', #8737, 3.000000000000000444 ) ;
#10212 = EDGE_LOOP ( 'NONE', ( #2812, #419, #7979, #3145, #7663 ) ) ;
#10213 = FACE_OUTER_BOUND ( 'NONE', #3164, .T. ) ;
#10214 = AXIS2_PLACEMENT_3D ( 'NONE', #435, #380, #6840 ) ;
#10215 = EDGE_LOOP ( 'NONE', ( #2040, #3799, #9192, #7065, #8686, #9548, #10328, #6584, #1054, #4867 ) ) ;
#10216 = DIRECTION ( 'NONE',  ( -1.020596576251801193E-17, -0.9879067010856511510, -0.1550495080613485399 ) ) ;
#10217 = ORIENTED_EDGE ( 'NONE', *, *, #1532, .T. ) ;
#10218 = EDGE_CURVE ( 'NONE', #7105, #6373, #2241, .T. ) ;
#10219 = DIRECTION ( 'NONE',  ( -0.000000000000000000, 1.000000000000000000, 0.000000000000000000 ) ) ;
#10220 = VERTEX_POINT ( 'NONE', #2344 ) ;
#10221 = VERTEX_POINT ( 'NONE', #10402 ) ;
#10222 = B_SPLINE_CURVE_WITH_KNOTS ( 'NONE', 3,
 ( #3477, #3635, #10004, #2037, #2834, #9958, #5265, #5222, #8504, #8349, #8454, #7711, #1143, #1884, #6066, #2778 ),
 .UNSPECIFIED., .F., .F.,
 ( 4, 2, 2, 2, 2, 2, 2, 4 ),
 ( 0.000000000000000000, 0.0003991717881400778088, 0.0007983435762801556175, 0.001197515364420233481, 0.001596687152560311235, 0.002395030728840411450, 0.002794202516980451908, 0.003193374305120491932 ),
 .UNSPECIFIED. ) ;
#10223 = CARTESIAN_POINT ( 'NONE',  ( -30.29350689640809335, 2.445795361565304815E-15, 20.00000000000002132 ) ) ;
#10224 = CARTESIAN_POINT ( 'NONE',  ( 27.15769640663936713, -133.1457019118818721, 27.15769640663938489 ) ) ;
#10225 = VECTOR ( 'NONE', #268, 1000.000000000000114 ) ;
#10226 = CARTESIAN_POINT ( 'NONE',  ( 33.55285093437175448, 29.14909237014566301, 12.50000000000000000 ) ) ;
#10227 = DIRECTION ( 'NONE',  ( 0.000000000000000000, 0.000000000000000000, 1.000000000000000000 ) ) ;
#10228 = CARTESIAN_POINT ( 'NONE',  ( 6.250000000000005329, 0.000000000000000000, 0.000000000000000000 ) ) ;
#10229 = CARTESIAN_POINT ( 'NONE',  ( -56.36957570605427037, 137.0132282531173473, -3.999999999999989786 ) ) ;
#10230 = DIRECTION ( 'NONE',  ( 1.387778780781445676E-16, -0.000000000000000000, -1.000000000000000000 ) ) ;
#10231 = ORIENTED_EDGE ( 'NONE', *, *, #429, .F. ) ;
#10232 = CIRCLE ( 'NONE', #4969, 4.000000000000000000 ) ;
#10233 = LINE ( 'NONE', #4452, #1466 ) ;
#10234 = AXIS2_PLACEMENT_3D ( 'NONE', #2260, #9416, #1414 ) ;
#10235 = VERTEX_POINT ( 'NONE', #7123 ) ;
#10236 = DIRECTION ( 'NONE',  ( -1.000000000000000000, 0.000000000000000000, 0.000000000000000000 ) ) ;
#10237 = LINE ( 'NONE', #8635, #8660 ) ;
#10238 = CARTESIAN_POINT ( 'NONE',  ( -50.00000000000002842, -135.1457019118818721, 26.62179802177713484 ) ) ;
#10239 = EDGE_CURVE ( 'NONE', #1722, #9506, #2908, .T. ) ;
#10240 = CARTESIAN_POINT ( 'NONE',  ( -16.29350689640809691, 65.65569765742554864, 0.000000000000000000 ) ) ;
#10241 = CIRCLE ( 'NONE', #9220, 7.999999999999996447 ) ;
#10242 = DIRECTION ( 'NONE',  ( 1.000000000000000000, -0.000000000000000000, -0.000000000000000000 ) ) ;
#10243 = ORIENTED_EDGE ( 'NONE', *, *, #10176, .T. ) ;
#10244 = ORIENTED_EDGE ( 'NONE', *, *, #9365, .T. ) ;
#10245 = ORIENTED_EDGE ( 'NONE', *, *, #5786, .F. ) ;
#10246 = VERTEX_POINT ( 'NONE', #699 ) ;
#10247 = CARTESIAN_POINT ( 'NONE',  ( -168.7559887226706223, 267.8293446334838563, 0.000000000000000000 ) ) ;
#10248 = DIRECTION ( 'NONE',  ( 0.000000000000000000, 1.000000000000000000, -0.000000000000000000 ) ) ;
#10249 = AXIS2_PLACEMENT_3D ( 'NONE', #7678, #2794, #2903 ) ;
#10250 = CARTESIAN_POINT ( 'NONE',  ( -7.293506896408097795, 120.5696653505793705, 20.00000000000000711 ) ) ;
#10251 = CARTESIAN_POINT ( 'NONE',  ( 73.53765631853929108, 70.39106037767955115, 25.00000000000000000 ) ) ;
#10252 = EDGE_CURVE ( 'NONE', #3180, #2069, #6368, .T. ) ;
#10253 = CARTESIAN_POINT ( 'NONE',  ( -27.85255513972543895, 64.37996872128307757, 7.750000000000002665 ) ) ;
#10254 = ORIENTED_EDGE ( 'NONE', *, *, #8994, .F. ) ;
#10255 = CARTESIAN_POINT ( 'NONE',  ( -38.96131932220313132, -3.319229491889264416, -2.232199717805851691 ) ) ;
#10256 = VERTEX_POINT ( 'NONE', #4620 ) ;
#10257 = LINE ( 'NONE', #2035, #467 ) ;
#10258 = VECTOR ( 'NONE', #3047, 1000.000000000000000 ) ;
#10259 = LINE ( 'NONE', #2994, #6891 ) ;
#10260 = CARTESIAN_POINT ( 'NONE',  ( 4.856471286862176662, 145.0444252872335937, 30.00000000000000355 ) ) ;
#10261 = ADVANCED_FACE ( 'NONE', ( #8856 ), #5947, .F. ) ;
#10262 = DIRECTION ( 'NONE',  ( 0.000000000000000000, 0.000000000000000000, 1.000000000000000000 ) ) ;
#10263 = EDGE_CURVE ( 'NONE', #10023, #4985, #1596, .T. ) ;
#10264 = VERTEX_POINT ( 'NONE', #5468 ) ;
#10265 = DIRECTION ( 'NONE',  ( 1.000000000000000000, -0.000000000000000000, -0.000000000000000000 ) ) ;
#10266 = VECTOR ( 'NONE', #10378, 1000.000000000000000 ) ;
#10267 = ORIENTED_EDGE ( 'NONE', *, *, #1053, .T. ) ;
#10268 = SHAPE_DEFINITION_REPRESENTATION ( #9504, #5068 ) ;
#10269 = ORIENTED_EDGE ( 'NONE', *, *, #2872, .F. ) ;
#10270 = TOROIDAL_SURFACE ( 'NONE', #3672, 24.24539146688411506, 5.000000000000000000 ) ;
#10271 = DIRECTION ( 'NONE',  ( -0.000000000000000000, -1.000000000000000000, -0.000000000000000000 ) ) ;
#10272 = ORIENTED_EDGE ( 'NONE', *, *, #4375, .F. ) ;
#10273 = ORIENTED_EDGE ( 'NONE', *, *, #9501, .T. ) ;
#10274 = CARTESIAN_POINT ( 'NONE',  ( -48.00000000000002132, -115.1457019118818863, 23.15769640663938134 ) ) ;
#10275 = DIRECTION ( 'NONE',  ( -6.485608039485835891E-17, -0.9063077870366466060, -0.4226182617407067132 ) ) ;
#10276 = EDGE_LOOP ( 'NONE', ( #6901, #7808, #8921, #10052 ) ) ;
#10277 = VECTOR ( 'NONE', #6417, 1000.000000000000000 ) ;
#10278 = DIRECTION ( 'NONE',  ( -1.000000000000000000, 0.000000000000000000, 0.000000000000000000 ) ) ;
#10279 = EDGE_CURVE ( 'NONE', #10221, #8048, #10192, .T. ) ;
#10280 = EDGE_CURVE ( 'NONE', #36, #2136, #206, .T. ) ;
#10281 = CYLINDRICAL_SURFACE ( 'NONE', #9749, 4.000000000000016875 ) ;
#10282 = CIRCLE ( 'NONE', #1635, 4.000000000000003553 ) ;
#10283 = EDGE_CURVE ( 'NONE', #6231, #3393, #10365, .T. ) ;
#10284 = DIRECTION ( 'NONE',  ( 1.734723475976806848E-16, 0.000000000000000000, 1.000000000000000000 ) ) ;
#10285 = DIRECTION ( 'NONE',  ( -1.000000000000000000, -0.000000000000000000, -0.000000000000000000 ) ) ;
#10286 = ORIENTED_EDGE ( 'NONE', *, *, #8882, .F. ) ;
#10287 = AXIS2_PLACEMENT_3D ( 'NONE', #9806, #4124, #5753 ) ;
#10288 = PLANE ( 'NONE',  #9076 ) ;
#10289 = VECTOR ( 'NONE', #1934, 1000.000000000000000 ) ;
#10290 = ORIENTED_EDGE ( 'NONE', *, *, #9363, .F. ) ;
#10291 = DIRECTION ( 'NONE',  ( -0.000000000000000000, 1.000000000000000000, -0.000000000000000000 ) ) ;
#10292 = DIRECTION ( 'NONE',  ( 0.000000000000000000, 0.000000000000000000, -1.000000000000000000 ) ) ;
#10293 = SHAPE_REPRESENTATION_RELATIONSHIP ( 'NONE' , 'NONE' ,  #3996, #2018 ) ;
#10294 = ORIENTED_EDGE ( 'NONE', *, *, #6467, .T. ) ;
#10295 = DIRECTION ( 'NONE',  ( 0.000000000000000000, 0.000000000000000000, -1.000000000000000000 ) ) ;
#10296 = FACE_OUTER_BOUND ( 'NONE', #8971, .T. ) ;
#10297 = VECTOR ( 'NONE', #5732, 1000.000000000000000 ) ;
#10298 = EDGE_CURVE ( 'NONE', #2542, #3031, #6266, .T. ) ;
#10299 = FACE_OUTER_BOUND ( 'NONE', #2206, .T. ) ;
#10300 = ORIENTED_EDGE ( 'NONE', *, *, #8186, .F. ) ;
#10301 = ORIENTED_EDGE ( 'NONE', *, *, #2415, .T. ) ;
#10302 = VECTOR ( 'NONE', #10080, 1000.000000000000000 ) ;
#10303 = EDGE_CURVE ( 'NONE', #3453, #8369, #4192, .T. ) ;
#10304 = CIRCLE ( 'NONE', #3874, 4.025000000000000355 ) ;
#10305 = ORIENTED_EDGE ( 'NONE', *, *, #1799, .T. ) ;
#10306 = EDGE_LOOP ( 'NONE', ( #824, #3120, #2092, #4301 ) ) ;
#10307 = DIRECTION ( 'NONE',  ( -0.000000000000000000, -0.000000000000000000, -1.000000000000000000 ) ) ;
#10308 = FACE_BOUND ( 'NONE', #7470, .T. ) ;
#10309 = DIRECTION ( 'NONE',  ( 0.6585271261848805180, -0.7525569905852198538, 0.000000000000000000 ) ) ;
#10310 = CARTESIAN_POINT ( 'NONE',  ( -8.000000000000000000, 1.871412446612461755, 0.8726539554219916450 ) ) ;
#10311 = CARTESIAN_POINT ( 'NONE',  ( 39.99999999999998579, -135.1457019118818721, -44.00000000000001421 ) ) ;
#10312 = ORIENTED_EDGE ( 'NONE', *, *, #2943, .F. ) ;
#10313 = CARTESIAN_POINT ( 'NONE',  ( 25.44550000000000978, 0.000000000000000000, 0.000000000000000000 ) ) ;
#10314 = VECTOR ( 'NONE', #5487, 1000.000000000000000 ) ;
#10315 = EDGE_CURVE ( 'NONE', #7036, #7666, #7651, .T. ) ;
#10316 = EDGE_LOOP ( 'NONE', ( #6153, #2637, #1946, #536, #741 ) ) ;
#10317 = PLANE ( 'NONE',  #2155 ) ;
#10318 = FACE_OUTER_BOUND ( 'NONE', #3159, .T. ) ;
#10319 = DIRECTION ( 'NONE',  ( 0.000000000000000000, 0.000000000000000000, -1.000000000000000000 ) ) ;
#10320 = DIRECTION ( 'NONE',  ( 1.387778780781445676E-16, 0.000000000000000000, -1.000000000000000000 ) ) ;
#10321 = MANIFOLD_SOLID_BREP ( 'Move Face3', #5368 ) ;
#10322 = VERTEX_POINT ( 'NONE', #4292 ) ;
#10323 = CARTESIAN_POINT ( 'NONE',  ( -30.29350689640809335, 150.5696653505793563, 0.000000000000000000 ) ) ;
#10324 = EDGE_LOOP ( 'NONE', ( #9222, #6017, #27, #5700 ) ) ;
#10325 = CARTESIAN_POINT ( 'NONE',  ( -56.36957570605427748, 150.5696653505793563, 10.90000000000000036 ) ) ;
#10326 = AXIS2_PLACEMENT_3D ( 'NONE', #2533, #6455, #3336 ) ;
#10327 = EDGE_CURVE ( 'NONE', #9114, #4137, #4763, .T. ) ;
#10328 = ORIENTED_EDGE ( 'NONE', *, *, #2583, .F. ) ;
#10329 = ORIENTED_EDGE ( 'NONE', *, *, #5397, .T. ) ;
#10330 = DIRECTION ( 'NONE',  ( 0.000000000000000000, 0.000000000000000000, 1.000000000000000000 ) ) ;
#10331 = CARTESIAN_POINT ( 'NONE',  ( 23.15769640663936713, -115.1457019118818863, 47.99999999999997868 ) ) ;
#10332 = CARTESIAN_POINT ( 'NONE',  ( -7.293506896408105789, 88.56966535057934209, 20.00000000000001066 ) ) ;
#10333 = DIRECTION ( 'NONE',  ( 1.000000000000000000, 0.000000000000000000, -0.000000000000000000 ) ) ;
#10334 = FACE_OUTER_BOUND ( 'NONE', #2867, .T. ) ;
#10335 = DIRECTION ( 'NONE',  ( 1.000000000000000000, 0.000000000000000000, 0.000000000000000000 ) ) ;
#10336 = CARTESIAN_POINT ( 'NONE',  ( -39.00436953563450970, 0.03089877619826473382, 3.555871974361681342 ) ) ;
#10337 = ORIENTED_EDGE ( 'NONE', *, *, #8449, .F. ) ;
#10338 = CARTESIAN_POINT ( 'NONE',  ( 42.22511195853869026, -135.1457019118818721, -30.00000000000000355 ) ) ;
#10339 = EDGE_CURVE ( 'NONE', #9488, #5863, #1060, .T. ) ;
#10340 = EDGE_CURVE ( 'NONE', #5302, #9869, #7476, .T. ) ;
#10341 = ADVANCED_FACE ( 'NONE', ( #3290 ), #2907, .T. ) ;
#10342 = ORIENTED_EDGE ( 'NONE', *, *, #8857, .T. ) ;
#10343 = DIRECTION ( 'NONE',  ( 1.000000000000000000, 3.469446951953610639E-15, -0.000000000000000000 ) ) ;
#10344 = CARTESIAN_POINT ( 'NONE',  ( -7.293506896408097795, 80.56966535057935630, 20.00000000000000711 ) ) ;
#10345 = DIRECTION ( 'NONE',  ( 1.000000000000000000, 0.000000000000000000, 0.000000000000000000 ) ) ;
#10346 = DIRECTION ( 'NONE',  ( 0.000000000000000000, 1.431206729101514631E-16, 1.000000000000000000 ) ) ;
#10347 = CARTESIAN_POINT ( 'NONE',  ( 6.250000000000005329, 0.000000000000000000, 0.000000000000000000 ) ) ;
#10348 = ORIENTED_EDGE ( 'NONE', *, *, #32, .F. ) ;
#10349 = ORIENTED_EDGE ( 'NONE', *, *, #8317, .F. ) ;
#10350 = EDGE_LOOP ( 'NONE', ( #9561, #219, #5812, #301, #3887, #4034, #7013, #10011 ) ) ;
#10351 = ADVANCED_FACE ( 'NONE', ( #2600 ), #2396, .F. ) ;
#10352 = EDGE_LOOP ( 'NONE', ( #8914, #10217 ) ) ;
#10353 = CARTESIAN_POINT ( 'NONE',  ( -50.00000000000001421, -134.3099331815685389, -24.41868145091762798 ) ) ;
#10354 = CIRCLE ( 'NONE', #8649, 3.297986701801175258 ) ;
#10355 = CARTESIAN_POINT ( 'NONE',  ( -1.071796769724492338, -3.319229491889267081, -2.232199717805850803 ) ) ;
#10356 = DIRECTION ( 'NONE',  ( 0.000000000000000000, 0.4226182617407066577, -0.9063077870366466060 ) ) ;
#10357 = FACE_OUTER_BOUND ( 'NONE', #1373, .T. ) ;
#10358 = ORIENTED_EDGE ( 'NONE', *, *, #2487, .T. ) ;
#10359 = DIRECTION ( 'NONE',  ( 0.000000000000000000, 0.000000000000000000, 1.000000000000000000 ) ) ;
#10360 = AXIS2_PLACEMENT_3D ( 'NONE', #1349, #4730, #705 ) ;
#10361 = CIRCLE ( 'NONE', #7983, 10.00000000000000178 ) ;
#10362 = EDGE_LOOP ( 'NONE', ( #10199, #9312, #9872, #3371 ) ) ;
#10363 = FACE_BOUND ( 'NONE', #6887, .T. ) ;
#10364 = PLANE ( 'NONE',  #5533 ) ;
#10365 = CIRCLE ( 'NONE', #4928, 4.025000000000000355 ) ;
#10366 = DIRECTION ( 'NONE',  ( -0.000000000000000000, -0.000000000000000000, -1.000000000000000000 ) ) ;
#10367 = EDGE_CURVE ( 'NONE', #3381, #7949, #8826, .T. ) ;
#10368 = CARTESIAN_POINT ( 'NONE',  ( -2.293506896408097795, 37.08684478514406635, -15.00000000000000355 ) ) ;
#10369 = ORIENTED_EDGE ( 'NONE', *, *, #655, .F. ) ;
#10370 = CARTESIAN_POINT ( 'NONE',  ( 73.53765631853929108, 70.39106037767953694, -30.00000000000000355 ) ) ;
#10371 = DIRECTION ( 'NONE',  ( 1.000000000000000000, 0.000000000000000000, 6.762231606186668710E-17 ) ) ;
#10372 = VERTEX_POINT ( 'NONE', #6679 ) ;
#10373 = AXIS2_PLACEMENT_3D ( 'NONE', #8010, #9511, #2243 ) ;
#10374 = CARTESIAN_POINT ( 'NONE',  ( -40.00000000000001421, -135.1457019118818721, -40.00000000000002132 ) ) ;
#10375 = AXIS2_PLACEMENT_3D ( 'NONE', #5064, #7509, #5751 ) ;
#10376 = ORIENTED_EDGE ( 'NONE', *, *, #772, .T. ) ;
#10377 = ORIENTED_EDGE ( 'NONE', *, *, #3719, .T. ) ;
#10378 = DIRECTION ( 'NONE',  ( 0.000000000000000000, 0.000000000000000000, -1.000000000000000000 ) ) ;
#10379 = DIRECTION ( 'NONE',  ( 1.000000000000000000, 0.000000000000000000, 0.000000000000000000 ) ) ;
#10380 = LINE ( 'NONE', #6241, #9057 ) ;
#10381 = ADVANCED_BREP_SHAPE_REPRESENTATION ( '', ( #3161, #4601 ), #8362 ) ;
#10382 = AXIS2_PLACEMENT_3D ( 'NONE', #2875, #2078, #5308 ) ;
#10383 = PLANE ( 'NONE',  #4418 ) ;
#10384 = CARTESIAN_POINT ( 'NONE',  ( -48.00000000000002132, -117.1457019118819005, -23.15769640663945594 ) ) ;
#10385 = EDGE_CURVE ( 'NONE', #3749, #7484, #4262, .T. ) ;
#10386 = CIRCLE ( 'NONE', #2593, 4.025000000000000355 ) ;
#10387 = ORIENTED_EDGE ( 'NONE', *, *, #8967, .F. ) ;
#10388 = CARTESIAN_POINT ( 'NONE',  ( 39.99999999999998579, -145.1457019118819005, -40.00000000000002132 ) ) ;
#10389 = EDGE_LOOP ( 'NONE', ( #569, #3201, #6983, #8998, #319, #8545, #10006, #6152, #3332, #1014 ) ) ;
#10390 = CARTESIAN_POINT ( 'NONE',  ( -2.293506896408097795, 120.5696653505793705, 28.00000000000000355 ) ) ;
#10391 = CARTESIAN_POINT ( 'NONE',  ( -11.29350689640808802, 105.5289575273812233, 54.43095569077609497 ) ) ;
#10392 = DIRECTION ( 'NONE',  ( 0.000000000000000000, -1.000000000000000000, 0.000000000000000000 ) ) ;
#10393 = DIRECTION ( 'NONE',  ( 1.000000000000000000, 0.000000000000000000, -2.154935995002246132E-16 ) ) ;
#10394 = EDGE_LOOP ( 'NONE', ( #4669, #754, #1778, #6452, #3307, #982, #5385 ) ) ;
#10395 = EDGE_CURVE ( 'NONE', #7038, #8587, #3423, .T. ) ;
#10396 = TOROIDAL_SURFACE ( 'NONE', #4125, 4.000000000000000000, 2.000000000000000000 ) ;
#10397 = ADVANCED_FACE ( 'NONE', ( #5087 ), #8911, .T. ) ;
#10398 = EDGE_CURVE ( 'NONE', #5542, #991, #267, .T. ) ;
#10399 = ORIENTED_EDGE ( 'NONE', *, *, #5905, .F. ) ;
#10400 = EDGE_LOOP ( 'NONE', ( #8130, #6095, #7780, #5809 ) ) ;
#10401 = CARTESIAN_POINT ( 'NONE',  ( -50.00000000000001421, -135.0799163051958942, -25.93999053166059099 ) ) ;
#10402 = CARTESIAN_POINT ( 'NONE',  ( -25.15769640663939199, -117.1457019118819005, -27.15769640663944173 ) ) ;
#10403 = CARTESIAN_POINT ( 'NONE',  ( -121.7299640054770578, 230.8694527092982867, 0.000000000000000000 ) ) ;
#10404 = CARTESIAN_POINT ( 'NONE',  ( -142.3328939341254795, 249.4204141414382434, 0.000000000000000000 ) ) ;
#10405 = PRODUCT_RELATED_PRODUCT_CATEGORY ( 'part', '', ( #2472 ) ) ;
#10406 = CARTESIAN_POINT ( 'NONE',  ( 39.99999999999998579, -115.1457019118818863, -40.00000000000002132 ) ) ;
#10407 = EDGE_CURVE ( 'NONE', #6075, #4224, #9823, .T. ) ;
#10408 = EDGE_CURVE ( 'NONE', #8958, #9336, #2062, .T. ) ;
#10409 = ORIENTED_EDGE ( 'NONE', *, *, #1581, .T. ) ;
#10410 = DIRECTION ( 'NONE',  ( 1.000000000000000000, 0.000000000000000000, 0.000000000000000000 ) ) ;
#10411 = AXIS2_PLACEMENT_3D ( 'NONE', #10469, #8871, #1561 ) ;
#10412 = ORIENTED_EDGE ( 'NONE', *, *, #9980, .F. ) ;
#10413 = AXIS2_PLACEMENT_3D ( 'NONE', #8149, #9919, #5869 ) ;
#10414 = CARTESIAN_POINT ( 'NONE',  ( 10.26554134690924691, 64.37996872128307757, 7.749999999999998224 ) ) ;
#10415 = CARTESIAN_POINT ( 'NONE',  ( -16.29350689640809691, -186.9457019118818835, -27.01918567566963247 ) ) ;
#10416 = CARTESIAN_POINT ( 'NONE',  ( 37.22759939293836595, -116.8755810935459323, 25.15769640663938489 ) ) ;
#10417 = CIRCLE ( 'NONE', #1452, 70.74985237403969052 ) ;
#10418 = EDGE_CURVE ( 'NONE', #9202, #7171, #8477, .T. ) ;
#10419 = VERTEX_POINT ( 'NONE', #3716 ) ;
#10420 = CARTESIAN_POINT ( 'NONE',  ( -40.00000000000002842, -135.1707019118818778, 39.99999999999997868 ) ) ;
#10421 = PRODUCT_CONTEXT ( 'NONE', #4628, 'mechanical' ) ;
#10422 = ORIENTED_EDGE ( 'NONE', *, *, #128, .T. ) ;
#10423 = CARTESIAN_POINT ( 'NONE',  ( -2.293506896408097795, 120.5696653505793705, -16.00000000000000711 ) ) ;
#10424 = ORIENTED_EDGE ( 'NONE', *, *, #1380, .T. ) ;
#10425 = EDGE_CURVE ( 'NONE', #9180, #5994, #481, .T. ) ;
#10426 = VECTOR ( 'NONE', #7712, 1000.000000000000000 ) ;
#10427 = EDGE_LOOP ( 'NONE', ( #7471, #10300 ) ) ;
#10428 = CARTESIAN_POINT ( 'NONE',  ( -20.29350689640809691, 140.5696653505793563, 10.98204862120179826 ) ) ;
#10429 = DIRECTION ( 'NONE',  ( 0.000000000000000000, 0.000000000000000000, 1.000000000000000000 ) ) ;
#10430 = CARTESIAN_POINT ( 'NONE',  ( -16.29350689640809691, 11.33971203780352255, 0.000000000000000000 ) ) ;
#10431 = DIRECTION ( 'NONE',  ( 1.396588258780021135E-16, 0.000000000000000000, -1.000000000000000000 ) ) ;
#10432 = AXIS2_PLACEMENT_3D ( 'NONE', #7984, #2267, #3962 ) ;
#10433 = DIRECTION ( 'NONE',  ( 0.000000000000000000, -0.000000000000000000, 1.000000000000000000 ) ) ;
#10434 = CARTESIAN_POINT ( 'NONE',  ( -39.65624476065125492, 3.117691453623999909, -1.799999999999972955 ) ) ;
#10435 = PRODUCT_DEFINITION_SHAPE ( 'NONE', 'NONE',  #1785 ) ;
#10436 = AXIS2_PLACEMENT_3D ( 'NONE', #5105, #7546, #1027 ) ;
#10437 = EDGE_LOOP ( 'NONE', ( #7433, #5240, #5293, #10337 ) ) ;
#10438 = DIRECTION ( 'NONE',  ( -0.7431448254773957984, 0.6691306063588565722, -0.000000000000000000 ) ) ;
#10439 = VECTOR ( 'NONE', #9455, 1000.000000000000000 ) ;
#10440 = EDGE_LOOP ( 'NONE', ( #5591, #5168, #4882, #1770 ) ) ;
#10441 = DIRECTION ( 'NONE',  ( 0.000000000000000000, 0.000000000000000000, 1.000000000000000000 ) ) ;
#10442 = CARTESIAN_POINT ( 'NONE',  ( -30.29350689640809335, 80.56966535057935630, -20.00000000000000711 ) ) ;
#10443 = AXIS2_PLACEMENT_3D ( 'NONE', #5601, #5554, #683 ) ;
#10444 = DIRECTION ( 'NONE',  ( 0.000000000000000000, 0.000000000000000000, 1.000000000000000000 ) ) ;
#10445 = DIRECTION ( 'NONE',  ( 1.000000000000000000, -0.000000000000000000, -0.000000000000000000 ) ) ;
#10446 = DIRECTION ( 'NONE',  ( 0.000000000000000000, 0.000000000000000000, 1.000000000000000000 ) ) ;
#10447 = VERTEX_POINT ( 'NONE', #7688 ) ;
#10448 = AXIS2_PLACEMENT_3D ( 'NONE', #568, #6981, #3803 ) ;
#10449 = ORIENTED_EDGE ( 'NONE', *, *, #5667, .T. ) ;
#10450 = ORIENTED_EDGE ( 'NONE', *, *, #9442, .F. ) ;
#10451 = ORIENTED_EDGE ( 'NONE', *, *, #6119, .F. ) ;
#10452 = ADVANCED_FACE ( 'NONE', ( #2913 ), #1221, .T. ) ;
#10453 = CARTESIAN_POINT ( 'NONE',  ( -50.00000000000001421, -135.1457019118818721, -26.27514770175552528 ) ) ;
#10454 = DIRECTION ( 'NONE',  ( 0.000000000000000000, 0.000000000000000000, -1.000000000000000000 ) ) ;
#10455 = AXIS2_PLACEMENT_3D ( 'NONE', #7490, #5837, #4205 ) ;
#10456 = CARTESIAN_POINT ( 'NONE',  ( -48.00000000000002132, -115.1457019118818863, -23.15769640663945594 ) ) ;
#10457 = CARTESIAN_POINT ( 'NONE',  ( -47.94539818030330025, 137.0132282531173473, 3.999999999999991562 ) ) ;
#10458 = AXIS2_PLACEMENT_3D ( 'NONE', #5405, #6896, #1277 ) ;
#10459 = CARTESIAN_POINT ( 'NONE',  ( 80.08610854271792334, 54.73418909528891874, 25.00000000000000000 ) ) ;
#10460 = ORIENTED_EDGE ( 'NONE', *, *, #3081, .F. ) ;
#10461 = DIRECTION ( 'NONE',  ( -0.6691306063588564612, -0.7431448254773956874, 0.000000000000000000 ) ) ;
#10462 = VECTOR ( 'NONE', #6907, 1000.000000000000000 ) ;
#10463 = ORIENTED_EDGE ( 'NONE', *, *, #3146, .F. ) ;
#10464 = ADVANCED_FACE ( 'NONE', ( #4507 ), #3243, .F. ) ;
#10465 = CARTESIAN_POINT ( 'NONE',  ( 6.250000000000005329, 0.000000000000000000, 0.000000000000000000 ) ) ;
#10466 = EDGE_CURVE ( 'NONE', #1746, #10256, #4095, .T. ) ;
#10467 = ADVANCED_FACE ( 'NONE', ( #10182 ), #9169, .T. ) ;
#10468 = CIRCLE ( 'NONE', #7418, 4.000000000000000000 ) ;
#10469 = CARTESIAN_POINT ( 'NONE',  ( -16.29350689640809691, -115.1457019118818863, -27.01918567566963247 ) ) ;
#10470 = DIRECTION ( 'NONE',  ( 0.000000000000000000, -1.000000000000000000, -0.000000000000000000 ) ) ;
#10471 = ORIENTED_EDGE ( 'NONE', *, *, #7483, .T. ) ;
#10472 = DIRECTION ( 'NONE',  ( 0.000000000000000000, -1.000000000000000000, 0.000000000000000000 ) ) ;
#10473 = ORIENTED_EDGE ( 'NONE', *, *, #1140, .T. ) ;
#10474 = AXIS2_PLACEMENT_3D ( 'NONE', #1685, #7305, #50 ) ;
#10475 = LINE ( 'NONE', #8823, #2515 ) ;
#10476 = EDGE_LOOP ( 'NONE', ( #5483, #3253, #4175, #9024, #1827, #232 ) ) ;
#10477 = EDGE_CURVE ( 'NONE', #1722, #7036, #3502, .T. ) ;
#10478 = PLANE ( 'NONE',  #8321 ) ;
#10479 = NEXT_ASSEMBLY_USAGE_OCCURRENCE ( 'NAUO1', ' ', ' ', #3989, #9302, $ ) ;
#10480 = NEXT_ASSEMBLY_USAGE_OCCURRENCE ( 'NAUO2', ' ', ' ', #3989, #6773, $ ) ;
#10481 = NEXT_ASSEMBLY_USAGE_OCCURRENCE ( 'NAUO3', ' ', ' ', #3989, #3203, $ ) ;
#10482 = NEXT_ASSEMBLY_USAGE_OCCURRENCE ( 'NAUO4', ' ', ' ', #3989, #687, $ ) ;
#10483 = NEXT_ASSEMBLY_USAGE_OCCURRENCE ( 'NAUO5', ' ', ' ', #3989, #8329, $ ) ;
#10484 = NEXT_ASSEMBLY_USAGE_OCCURRENCE ( 'NAUO6', ' ', ' ', #3989, #1785, $ ) ;
#10485 = NEXT_ASSEMBLY_USAGE_OCCURRENCE ( 'NAUO7', ' ', ' ', #3989, #8197, $ ) ;
#10486 = NEXT_ASSEMBLY_USAGE_OCCURRENCE ( 'NAUO8', ' ', ' ', #3989, #8524, $ ) ;
#10487 = NEXT_ASSEMBLY_USAGE_OCCURRENCE ( 'NAUO9', ' ', ' ', #3989, #6322, $ ) ;
#10488 = NEXT_ASSEMBLY_USAGE_OCCURRENCE ( 'NAUO10', ' ', ' ', #3989, #6322, $ ) ;
#10489 = NEXT_ASSEMBLY_USAGE_OCCURRENCE ( 'NAUO11', ' ', ' ', #3989, #6322, $ ) ;
#10490 = NEXT_ASSEMBLY_USAGE_OCCURRENCE ( 'NAUO12', ' ', ' ', #3989, #6322, $ ) ;
#10491=COLOUR_RGB('Dark Blue',0.08,0.2,0.34);
#10492=FILL_AREA_STYLE_COLOUR('',#10491);
#10493=FILL_AREA_STYLE('',(#10492));
#10494=SURFACE_STYLE_FILL_AREA(#10493);
#10495=SURFACE_SIDE_STYLE('',(#10494));
#10496=SURFACE_STYLE_USAGE(.BOTH.,#10495);
#10497=PRESENTATION_STYLE_ASSIGNMENT((#10496));
#10498=COLOUR_RGB('Light Blue',0.38,0.62,0.78);
#10499=FILL_AREA_STYLE_COLOUR('',#10498);
#10500=FILL_AREA_STYLE('',(#10499));
#10501=SURFACE_STYLE_FILL_AREA(#10500);
#10502=SURFACE_SIDE_STYLE('',(#10501));
#10503=SURFACE_STYLE_USAGE(.BOTH.,#10502);
#10504=PRESENTATION_STYLE_ASSIGNMENT((#10503));
#10505=COLOUR_RGB('Sky Blue',0.24,0.69,0.87);
#10506=FILL_AREA_STYLE_COLOUR('',#10505);
#10507=FILL_AREA_STYLE('',(#10506));
#10508=SURFACE_STYLE_FILL_AREA(#10507);
#10509=SURFACE_SIDE_STYLE('',(#10508));
#10510=SURFACE_STYLE_USAGE(.BOTH.,#10509);
#10511=PRESENTATION_STYLE_ASSIGNMENT((#10510));
#10512=COLOUR_RGB('Grey',0.48,0.52,0.57);
#10513=FILL_AREA_STYLE_COLOUR('',#10512);
#10514=FILL_AREA_STYLE('',(#10513));
#10515=SURFACE_STYLE_FILL_AREA(#10514);
#10516=SURFACE_SIDE_STYLE('',(#10515));
#10517=SURFACE_STYLE_USAGE(.BOTH.,#10516);
#10518=PRESENTATION_STYLE_ASSIGNMENT((#10517));
#10519=COLOUR_RGB('Black',0.12,0.14,0.17);
#10520=FILL_AREA_STYLE_COLOUR('',#10519);
#10521=FILL_AREA_STYLE('',(#10520));
#10522=SURFACE_STYLE_FILL_AREA(#10521);
#10523=SURFACE_SIDE_STYLE('',(#10522));
#10524=SURFACE_STYLE_USAGE(.BOTH.,#10523);
#10525=PRESENTATION_STYLE_ASSIGNMENT((#10524));
#10526=COLOUR_RGB('Off White',0.89,0.88,0.83);
#10527=FILL_AREA_STYLE_COLOUR('',#10526);
#10528=FILL_AREA_STYLE('',(#10527));
#10529=SURFACE_STYLE_FILL_AREA(#10528);
#10530=SURFACE_SIDE_STYLE('',(#10529));
#10531=SURFACE_STYLE_USAGE(.BOTH.,#10530);
#10532=PRESENTATION_STYLE_ASSIGNMENT((#10531));
ENDSEC;
END-ISO-10303-21;
